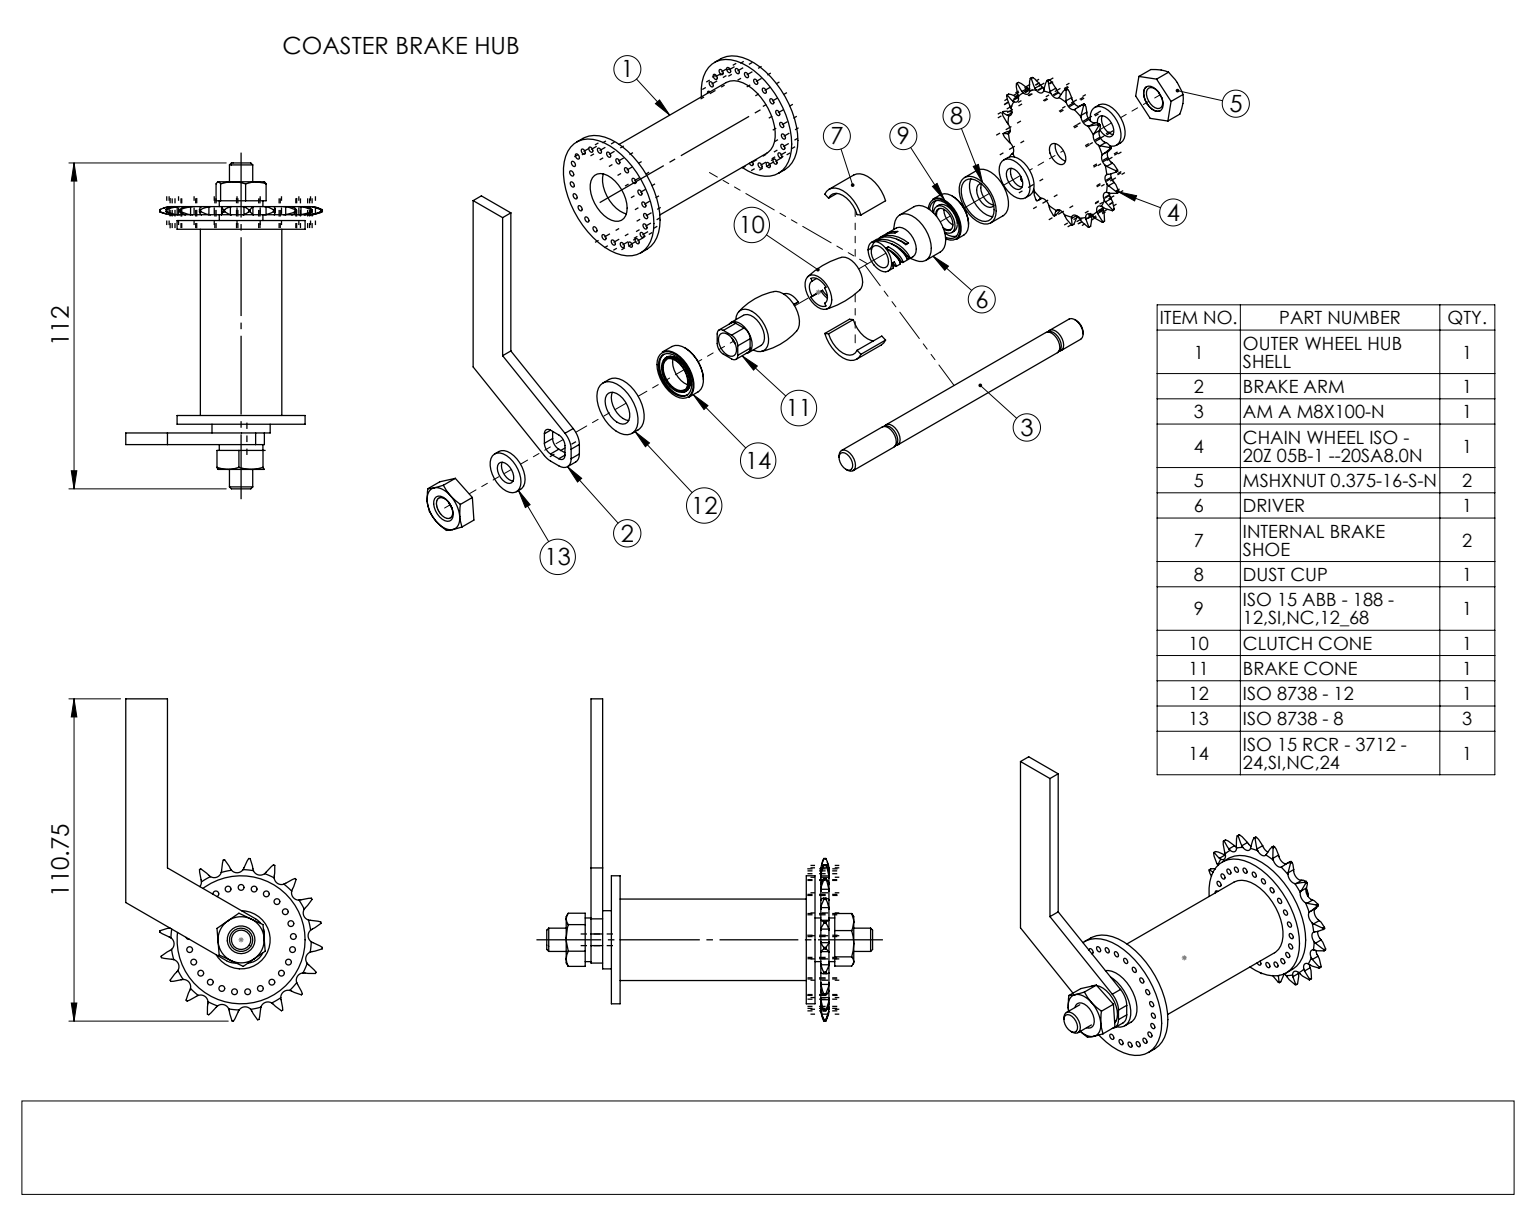
ISO-10303-21;
HEADER;
FILE_DESCRIPTION (('STEP AP214'),
    '1' );
FILE_NAME ('BR-591',
    '2026-10-08T05:56:58',
    ( '' ),
    ( '' ),
    'SwSTEP 2.0',
    'SolidWorks 2026',
    '' );
FILE_SCHEMA (( 'AUTOMOTIVE_DESIGN' ));
ENDSEC;

DATA;
#1 = ORIENTED_EDGE ( 'NONE', *, *, #18394, .T. ) ;
#2 = CARTESIAN_POINT ( 'NONE',  ( 0.07186808533286707934, 10.24630254990548650, -23.19485392143201707 ) ) ;
#3 = AXIS2_PLACEMENT_3D ( 'NONE', #18095, #1186, #4385 ) ;
#4 = FACE_OUTER_BOUND ( 'NONE', #5916, .T. ) ;
#5 = VECTOR ( 'NONE', #6897, 1000.000000000000000 ) ;
#6 = ORIENTED_EDGE ( 'NONE', *, *, #9270, .F. ) ;
#7 = CARTESIAN_POINT ( 'NONE',  ( 9.343749997951615427, -3.499494075959840966, 3.499494075959791672 ) ) ;
#8 = EDGE_CURVE ( 'NONE', #13643, #9700, #6131, .T. ) ;
#9 = CARTESIAN_POINT ( 'NONE',  ( 2.257825462012207574, 23.74442027961379864, -12.96514671151741638 ) ) ;
#10 = ORIENTED_EDGE ( 'NONE', *, *, #9147, .T. ) ;
#11 = ADVANCED_FACE ( 'NONE', ( #15453 ), #13841, .T. ) ;
#12 = CARTESIAN_POINT ( 'NONE',  ( 1.510506337161861223, 4.648860486681953397, -12.84374999795161543 ) ) ;
#13 = CARTESIAN_POINT ( 'NONE',  ( -15.00000000000000355, 4.874999999999997335, -3.903123748999000053 ) ) ;
#14 = ADVANCED_FACE ( 'NONE', ( #14340, #12840 ), #18938, .T. ) ;
#15 = VERTEX_POINT ( 'NONE', #17446 ) ;
#16 = VECTOR ( 'NONE', #6986, 1000.000000000000000 ) ;
#17 = B_SPLINE_CURVE_WITH_KNOTS ( 'NONE', 3,
 ( #2444, #6941, #2258, #8559, #14668, #14761 ),
 .UNSPECIFIED., .F., .F.,
 ( 4, 2, 4 ),
 ( 4.462636731831954487E-07, 0.001879885066974966781, 0.003759323870276750149 ),
 .UNSPECIFIED. ) ;
#18 = CARTESIAN_POINT ( 'NONE',  ( 12.84374999795161543, 1.016293382781411792, 4.781284448697195266 ) ) ;
#19 = CARTESIAN_POINT ( 'NONE',  ( 2.789999999999999147, -23.17675759782046541, 7.772527002114348882 ) ) ;
#20 = EDGE_LOOP ( 'NONE', ( #15641, #11996, #7928, #5193 ) ) ;
#21 = CARTESIAN_POINT ( 'NONE',  ( -14.19790265903626647, 9.644882309621941374, 35.00000000000000000 ) ) ;
#22 = VERTEX_POINT ( 'NONE', #14244 ) ;
#23 = CARTESIAN_POINT ( 'NONE',  ( -5.313169144388804277, -6.097875887622428159, -0.08160424337824753738 ) ) ;
#24 = ORIENTED_EDGE ( 'NONE', *, *, #5256, .T. ) ;
#25 = CYLINDRICAL_SURFACE ( 'NONE', #12194, 5.400000000000000355 ) ;
#26 = ADVANCED_FACE ( 'NONE', ( #15747 ), #18840, .T. ) ;
#27 = DIRECTION ( 'NONE',  ( 0.000000000000000000, 0.000000000000000000, 1.000000000000000000 ) ) ;
#28 = CARTESIAN_POINT ( 'NONE',  ( -10.58013454126452224, -14.56230589874905235, 32.00000000000000000 ) ) ;
#29 = CARTESIAN_POINT ( 'NONE',  ( -41.99999999999999289, -2.000000000000001776, 5.000000000000000000 ) ) ;
#30 = ORIENTED_EDGE ( 'NONE', *, *, #18526, .T. ) ;
#31 = CARTESIAN_POINT ( 'NONE',  ( 2.789999999999999147, -24.34211360614294506, -7.909232158575071558 ) ) ;
#32 =( BOUNDED_CURVE ( )  B_SPLINE_CURVE ( 2, ( #2369, #8482, #14588, #875, #19172, #5461, #16578, #8772, #11868, #7343, #19367, #11771, #17980, #5752, #6052 ),
 .UNSPECIFIED., .F., .F. ) 
 B_SPLINE_CURVE_WITH_KNOTS ( ( 3, 2, 2, 2, 2, 2, 2, 3 ),
 ( 0.000000000000000000, 0.05000000000000000278, 0.1000000000000000056, 0.1499999999999999944, 0.2000000000000000111, 0.2500000000000000000, 0.2999999999999999889, 0.3333180920165871863 ),
 .UNSPECIFIED. ) 
 CURVE ( )  GEOMETRIC_REPRESENTATION_ITEM ( )  RATIONAL_B_SPLINE_CURVE ( ( 1.000000000000000000, 0.9876883405951377704, 1.000000000000000000, 0.9876883405951377704, 1.000000000000000000, 0.9876883405951377704, 1.000000000000000000, 0.9876883405951377704, 1.000000000000000000, 0.9876883405951377704, 1.000000000000000000, 0.9876883405951377704, 1.000000000000000000, 0.9917959799814384247, 0.9945256517182510247 ) ) 
 REPRESENTATION_ITEM ( '' )  );
#33 = AXIS2_PLACEMENT_3D ( 'NONE', #19448, #5737, #11851 ) ;
#34 =( REPRESENTATION_RELATIONSHIP ('NONE','NONE', #18211, #17568 ) REPRESENTATION_RELATIONSHIP_WITH_TRANSFORMATION ( #11544 )SHAPE_REPRESENTATION_RELATIONSHIP( ) );
#35 = ADVANCED_FACE ( 'NONE', ( #2227 ), #2033, .F. ) ;
#36 = SURFACE_STYLE_FILL_AREA ( #16650 ) ;
#37 = CARTESIAN_POINT ( 'NONE',  ( -5.207209108562804722, 2.318398865532109276, -15.31249999590322552 ) ) ;
#38 = CARTESIAN_POINT ( 'NONE',  ( 15.28688694438835505, -7.664027248171309203, -32.00000000000000000 ) ) ;
#39 = DIRECTION ( 'NONE',  ( -1.000000000000000000, -0.000000000000000000, -0.000000000000000000 ) ) ;
#40 = ORIENTED_EDGE ( 'NONE', *, *, #11273, .T. ) ;
#41 = DIRECTION ( 'NONE',  ( 0.000000000000000000, 1.224646799147353454E-16, 1.000000000000000000 ) ) ;
#42 = ADVANCED_FACE ( 'NONE', ( #15944 ), #11240, .F. ) ;
#43 = DIRECTION ( 'NONE',  ( 1.000000000000000000, 0.000000000000000000, 0.000000000000000000 ) ) ;
#44 = ORIENTED_EDGE ( 'NONE', *, *, #4692, .F. ) ;
#45 = DIRECTION ( 'NONE',  ( 0.000000000000000000, 0.000000000000000000, -1.000000000000000000 ) ) ;
#46 = VECTOR ( 'NONE', #13444, 1000.000000000000000 ) ;
#47 = DIRECTION ( 'NONE',  ( 1.000000000000000000, 0.000000000000000000, 0.000000000000000000 ) ) ;
#48 = AXIS2_PLACEMENT_3D ( 'NONE', #1489, #16900, #7577 ) ;
#49 = DIRECTION ( 'NONE',  ( 0.000000000000000000, 0.000000000000000000, -1.000000000000000000 ) ) ;
#50 = CARTESIAN_POINT ( 'NONE',  ( -1.493657965219562511, -5.574407415329147852, -9.812499995903225525 ) ) ;
#51 = EDGE_CURVE ( 'NONE', #4769, #2089, #9336, .T. ) ;
#52 = CIRCLE ( 'NONE', #15065, 1.000000000000004441 ) ;
#53 = EDGE_LOOP ( 'NONE', ( #13652, #15680, #15664, #19409 ) ) ;
#54 = ORIENTED_EDGE ( 'NONE', *, *, #11125, .T. ) ;
#55 = CARTESIAN_POINT ( 'NONE',  ( 0.1882238782932349475, -17.47009390565476750, -19.18368891937510412 ) ) ;
#56 = CARTESIAN_POINT ( 'NONE',  ( 12.34374999795161543, 4.888101187500000222, 0.7741991708318884946 ) ) ;
#57 = ORIENTED_EDGE ( 'NONE', *, *, #11077, .F. ) ;
#58 = B_SPLINE_CURVE_WITH_KNOTS ( 'NONE', 3,
 ( #4738, #3235, #18159, #5934, #19743, #13850 ),
 .UNSPECIFIED., .F., .F.,
 ( 4, 2, 4 ),
 ( 4.462636882236601199E-07, 0.001879885203074806947, 0.003759324142461389993 ),
 .UNSPECIFIED. ) ;
#59 = VERTEX_POINT ( 'NONE', #14445 ) ;
#60 = FILL_AREA_STYLE ('',( #15279 ) ) ;
#61 = AXIS2_PLACEMENT_3D ( 'NONE', #11825, #841, #14548 ) ;
#62 = VERTEX_POINT ( 'NONE', #2132 ) ;
#63 = CIRCLE ( 'NONE', #5149, 40.00000000000000711 ) ;
#64 = VECTOR ( 'NONE', #5510, 1000.000000000000000 ) ;
#65 = AXIS2_PLACEMENT_3D ( 'NONE', #16794, #19682, #3071 ) ;
#66 = DIRECTION ( 'NONE',  ( -1.000000000000000000, 0.000000000000000000, 0.000000000000000000 ) ) ;
#67 = DIRECTION ( 'NONE',  ( -1.000000000000000000, 0.000000000000000000, 0.000000000000000000 ) ) ;
#68 = DIRECTION ( 'NONE',  ( 1.000000000000000000, 0.000000000000000000, 0.000000000000000000 ) ) ;
#69 = ORIENTED_EDGE ( 'NONE', *, *, #7451, .F. ) ;
#70 = ORIENTED_EDGE ( 'NONE', *, *, #8344, .T. ) ;
#71 = B_SPLINE_CURVE_WITH_KNOTS ( 'NONE', 3,
 ( #7909, #17128, #18622, #4920 ),
 .UNSPECIFIED., .F., .F.,
 ( 4, 4 ),
 ( 0.005258110598983589158, 0.005948376585272731332 ),
 .UNSPECIFIED. ) ;
#72 = CARTESIAN_POINT ( 'NONE',  ( 0.02436607992776411782, 22.71065055754465689, -9.836394144775473691 ) ) ;
#73 = DIRECTION ( 'NONE',  ( -1.000000000000000000, 0.000000000000000000, 0.000000000000000000 ) ) ;
#74 = EDGE_CURVE ( 'NONE', #13547, #344, #8025, .T. ) ;
#75 = ORIENTED_EDGE ( 'NONE', *, *, #12842, .F. ) ;
#76 = CARTESIAN_POINT ( 'NONE',  ( 2.789999999999999147, 19.64056340710875048, -14.55412442567624609 ) ) ;
#77 = AXIS2_PLACEMENT_3D ( 'NONE', #8605, #16216, #8311 ) ;
#78 = FACE_BOUND ( 'NONE', #16173, .T. ) ;
#79 = AXIS2_PLACEMENT_3D ( 'NONE', #11870, #19566, #2860 ) ;
#80 = CARTESIAN_POINT ( 'NONE',  ( 2.789999999999999147, -15.04425356660744839, -18.18163861606288378 ) ) ;
#81 = AXIS2_PLACEMENT_3D ( 'NONE', #18484, #1485, #6266 ) ;
#82 = CARTESIAN_POINT ( 'NONE',  ( 2.765633920072239516, 21.30679549418631780, 12.59161484032919986 ) ) ;
#83 = CARTESIAN_POINT ( 'NONE',  ( -4.620319390059805187, 1.773574444220790136, -11.34374999795161543 ) ) ;
#84 = EDGE_CURVE ( 'NONE', #8438, #18497, #5035, .T. ) ;
#85 = ORIENTED_EDGE ( 'NONE', *, *, #1576, .T. ) ;
#86 = DIRECTION ( 'NONE',  ( -0.9340060080012921873, 4.375140065418248206E-17, -0.3572572980605013271 ) ) ;
#87 = VECTOR ( 'NONE', #9663, 1000.000000000000000 ) ;
#88 = DIRECTION ( 'NONE',  ( 0.000000000000000000, 0.000000000000000000, -1.000000000000000000 ) ) ;
#89 = ORIENTED_EDGE ( 'NONE', *, *, #3339, .T. ) ;
#90 = PLANE ( 'NONE',  #2084 ) ;
#91 = CARTESIAN_POINT ( 'NONE',  ( 13.34374999795161365, -0.2590123213420631454, -4.942249507334558700 ) ) ;
#92 = AXIS2_PLACEMENT_3D ( 'NONE', #12278, #16979, #66 ) ;
#93 = EDGE_CURVE ( 'NONE', #2524, #1421, #17025, .T. ) ;
#94 = CARTESIAN_POINT ( 'NONE',  ( 8.468749997951615427, -1.988169868018530462, -4.465502636338051445 ) ) ;
#95 = DIRECTION ( 'NONE',  ( -1.000000000000000000, -0.000000000000000000, 0.000000000000000000 ) ) ;
#96 = ORIENTED_EDGE ( 'NONE', *, *, #17923, .T. ) ;
#97 = AXIS2_PLACEMENT_3D ( 'NONE', #19744, #12155, #18353 ) ;
#98 = CARTESIAN_POINT ( 'NONE',  ( 0.000000000000000000, 0.000000000000000000, -35.00000000000000000 ) ) ;
#99 = CYLINDRICAL_SURFACE ( 'NONE', #7805, 22.00000000000000355 ) ;
#100 = AXIS2_PLACEMENT_3D ( 'NONE', #5188, #8093, #8295 ) ;
#101 = CARTESIAN_POINT ( 'NONE',  ( 1.749999999999998002, -12.52377138324241734, 25.12109765559649688 ) ) ;
#102 = ORIENTED_EDGE ( 'NONE', *, *, #9565, .F. ) ;
#103 = CARTESIAN_POINT ( 'NONE',  ( -2.000000000000001776, 3.950217066951266176, 3.681818181818181213 ) ) ;
#104 = CARTESIAN_POINT ( 'NONE',  ( 11.46874999795161543, -2.444050593750019651, 4.233219804643871598 ) ) ;
#105 = CARTESIAN_POINT ( 'NONE',  ( 10.50000000000000711, 3.631840208645794821, 4.484949146646379781 ) ) ;
#106 = FACE_OUTER_BOUND ( 'NONE', #19772, .T. ) ;
#107 = EDGE_LOOP ( 'NONE', ( #13060, #5147, #11835, #11833, #16317, #5831 ) ) ;
#108 = CARTESIAN_POINT ( 'NONE',  ( 0.000000000000000000, 0.000000000000000000, 35.00000000000000000 ) ) ;
#109 = PRESENTATION_LAYER_ASSIGNMENT (  '', '', ( #8729 ) ) ;
#110 = CARTESIAN_POINT ( 'NONE',  ( 17.11901729331276556, 5.562305898749055011, -32.00000000000000000 ) ) ;
#111 = EDGE_CURVE ( 'NONE', #18625, #19430, #2327, .T. ) ;
#112 = EDGE_LOOP ( 'NONE', ( #14976, #17083 ) ) ;
#113 = FACE_OUTER_BOUND ( 'NONE', #17596, .T. ) ;
#114 = DIRECTION ( 'NONE',  ( -1.000000000000000000, -0.000000000000000000, -0.000000000000000000 ) ) ;
#115 = ORIENTED_EDGE ( 'NONE', *, *, #15621, .F. ) ;
#116 = AXIS2_PLACEMENT_3D ( 'NONE', #3393, #4893, #17196 ) ;
#117 = CARTESIAN_POINT ( 'NONE',  ( 1.749999999999998002, -4.633866840648726004, -27.68468304288263582 ) ) ;
#118 = CARTESIAN_POINT ( 'NONE',  ( -34.92499999999994742, 0.000000000000000000, 4.000000000000000000 ) ) ;
#119 = ORIENTED_EDGE ( 'NONE', *, *, #8237, .F. ) ;
#120 =( GEOMETRIC_REPRESENTATION_CONTEXT ( 3 ) GLOBAL_UNCERTAINTY_ASSIGNED_CONTEXT ( ( #987 ) ) GLOBAL_UNIT_ASSIGNED_CONTEXT ( ( #1597, #16819, #7588 ) ) REPRESENTATION_CONTEXT ( 'NONE', 'WORKASPACE' ) );
#121 = LINE ( 'NONE', #4819, #1475 ) ;
#122 = CARTESIAN_POINT ( 'NONE',  ( -34.92499999999994742, 0.000000000000000000, 0.000000000000000000 ) ) ;
#123 = VERTEX_POINT ( 'NONE', #15646 ) ;
#124 = EDGE_CURVE ( 'NONE', #6609, #1230, #1374, .T. ) ;
#125 = DIRECTION ( 'NONE',  ( -1.000000000000000000, -0.000000000000000000, -0.000000000000000000 ) ) ;
#126 = VERTEX_POINT ( 'NONE', #442 ) ;
#127 = EDGE_CURVE ( 'NONE', #15888, #11336, #18737, .T. ) ;
#128 = DIRECTION ( 'NONE',  ( 0.000000000000000000, 0.000000000000000000, 1.000000000000000000 ) ) ;
#129 = ORIENTED_EDGE ( 'NONE', *, *, #9030, .F. ) ;
#130 = DIRECTION ( 'NONE',  ( 1.000000000000000000, 0.000000000000000000, 0.000000000000000000 ) ) ;
#131 = AXIS2_PLACEMENT_3D ( 'NONE', #16442, #16336, #16243 ) ;
#132 = CARTESIAN_POINT ( 'NONE',  ( 2.631259771887293653, -22.38003579136350396, 12.81821841996065636 ) ) ;
#133 = DIRECTION ( 'NONE',  ( 1.000000000000000000, 0.000000000000000000, 0.000000000000000000 ) ) ;
#134 = EDGE_CURVE ( 'NONE', #16351, #5756, #19323, .T. ) ;
#135 = CARTESIAN_POINT ( 'NONE',  ( 0.1855656748306462045, -2.851997810081830842, 25.77772010606605235 ) ) ;
#136 = ORIENTED_EDGE ( 'NONE', *, *, #8190, .F. ) ;
#137 = DIRECTION ( 'NONE',  ( 0.000000000000000000, 0.000000000000000000, 1.000000000000000000 ) ) ;
#138 = PRESENTATION_LAYER_ASSIGNMENT (  '', '', ( #11327 ) ) ;
#139 = AXIS2_PLACEMENT_3D ( 'NONE', #2060, #12472, #13976 ) ;
#140 = LINE ( 'NONE', #6221, #2071 ) ;
#141 = EDGE_LOOP ( 'NONE', ( #3157, #7243, #2430, #12729, #17262, #10969 ) ) ;
#142 = VECTOR ( 'NONE', #16132, 1000.000000000000000 ) ;
#143 = DIRECTION ( 'NONE',  ( -0.000000000000000000, -0.000000000000000000, 1.000000000000000000 ) ) ;
#144 = CARTESIAN_POINT ( 'NONE',  ( 2.790000000000076419, -22.38018801136469094, -9.515416771311432598 ) ) ;
#145 = ORIENTED_EDGE ( 'NONE', *, *, #8344, .F. ) ;
#146 = CARTESIAN_POINT ( 'NONE',  ( 13.00000000000000533, 0.5958122406256767256, -5.668774803599153422 ) ) ;
#147 = CARTESIAN_POINT ( 'NONE',  ( 10.34374999795161543, 0.2590123213421660631, -4.942249507334553371 ) ) ;
#148 = ORIENTED_EDGE ( 'NONE', *, *, #16940, .F. ) ;
#149 = DIRECTION ( 'NONE',  ( 1.000000000000000000, 0.000000000000000000, -0.000000000000000000 ) ) ;
#150 = STYLED_ITEM ( 'NONE', ( #8512 ), #9431 ) ;
#151 = ORIENTED_EDGE ( 'NONE', *, *, #9100, .T. ) ;
#152 = SHAPE_DEFINITION_REPRESENTATION ( #11949, #13463 ) ;
#153 = CARTESIAN_POINT ( 'NONE',  ( 1.545624935189822177E-15, 9.165435523385314198, -6.527800000000000047 ) ) ;
#154 = CARTESIAN_POINT ( 'NONE',  ( -5.700000000000001066, -0.5990941410143296730, -13.64430100820692537 ) ) ;
#155 = VERTEX_POINT ( 'NONE', #3633 ) ;
#156 =( BOUNDED_SURFACE ( )  B_SPLINE_SURFACE ( 1, 2, ( 
 ( #19696, #12102, #10210, #2584, #16407, #18204, #1100, #2682, #8800, #7272, #189, #18685, #7680, #9499, #382, #3485, #10992 ),
 ( #15499, #9592, #10894, #9295, #13794, #4787, #17096, #10700, #6275, #4590, #15690, #10794, #17000, #15330, #18396, #284, #6461 ) ),
 .UNSPECIFIED., .F., .F., .F. ) 
 B_SPLINE_SURFACE_WITH_KNOTS ( ( 2, 2 ),
 ( 3, 2, 2, 2, 2, 2, 2, 2, 3 ),
 ( 0.000000000000000000, 1.000000000000000000 ),
 ( 0.000000000000000000, 0.05000000000000000278, 0.1000000000000000056, 0.1499999999999999944, 0.2000000000000000111, 0.2500000000000000000, 0.2999999999999999889, 0.3499999999999999778, 0.4000000000000000222 ),
 .UNSPECIFIED. ) 
 GEOMETRIC_REPRESENTATION_ITEM ( )  RATIONAL_B_SPLINE_SURFACE ( (
 ( 1.000000000000000000, 0.9876883405951377704, 1.000000000000000000, 0.9876883405951377704, 1.000000000000000000, 0.9876883405951377704, 1.000000000000000000, 0.9876883405951377704, 1.000000000000000000, 0.9876883405951377704, 1.000000000000000000, 0.9876883405951377704, 1.000000000000000000, 0.9876883405951377704, 1.000000000000000000, 0.9876883405951377704, 1.000000000000000000),
 ( 1.000000000000000000, 0.9876883405951377704, 1.000000000000000000, 0.9876883405951377704, 1.000000000000000000, 0.9876883405951377704, 1.000000000000000000, 0.9876883405951377704, 1.000000000000000000, 0.9876883405951377704, 1.000000000000000000, 0.9876883405951377704, 1.000000000000000000, 0.9876883405951377704, 1.000000000000000000, 0.9876883405951377704, 1.000000000000000000) ) ) 
 REPRESENTATION_ITEM ( '' )  SURFACE ( )  );
#157 = ORIENTED_EDGE ( 'NONE', *, *, #10548, .F. ) ;
#158 = CARTESIAN_POINT ( 'NONE',  ( -0.8944271909999155223, 0.000000000000000000, 0.000000000000000000 ) ) ;
#159 = CARTESIAN_POINT ( 'NONE',  ( 4.465502636338025688, -1.988169868018592412, -14.84374999795161543 ) ) ;
#161 = EDGE_LOOP ( 'NONE', ( #14576, #14310, #4192, #11228 ) ) ;
#160 = AXIS2_PLACEMENT_3D ( 'NONE', #12502, #14297, #392 ) ;
#162 = EDGE_CURVE ( 'NONE', #18627, #6765, #11284, .T. ) ;
#163 = EDGE_CURVE ( 'NONE', #5395, #4220, #13751, .T. ) ;
#164 = CYLINDRICAL_SURFACE ( 'NONE', #11252, 13.19999999999999929 ) ;
#165 = VECTOR ( 'NONE', #11258, 1000.000000000000000 ) ;
#166 = ORIENTED_EDGE ( 'NONE', *, *, #11587, .F. ) ;
#167 = EDGE_CURVE ( 'NONE', #11813, #19442, #2963, .T. ) ;
#168 = FACE_OUTER_BOUND ( 'NONE', #5426, .T. ) ;
#169 = CARTESIAN_POINT ( 'NONE',  ( 5.421022142882364392, -1.761396867937238486, -8.312499995903225525 ) ) ;
#170 = EDGE_CURVE ( 'NONE', #2370, #11052, #11954, .T. ) ;
#171 = ORIENTED_EDGE ( 'NONE', *, *, #6016, .T. ) ;
#172 = ORIENTED_EDGE ( 'NONE', *, *, #5127, .T. ) ;
#173 = CARTESIAN_POINT ( 'NONE',  ( -7.634507448887241432E-14, 22.38018801136490055, -9.515416771310970745 ) ) ;
#174 = EDGE_CURVE ( 'NONE', #16744, #5554, #14796, .T. ) ;
#175 = CARTESIAN_POINT ( 'NONE',  ( 6.234374998975811266, 0.000000000000000000, -5.294050593750000644 ) ) ;
#176 = ORIENTED_EDGE ( 'NONE', *, *, #9057, .T. ) ;
#177 = EDGE_LOOP ( 'NONE', ( #14869, #8807, #10159, #6951 ) ) ;
#178 = LINE ( 'NONE', #6262, #6325 ) ;
#179 = VECTOR ( 'NONE', #5539, 1000.000000000000000 ) ;
#180 = CARTESIAN_POINT ( 'NONE',  ( -5.387740456496247887, -2.068159791354146293, -12.81249999590322552 ) ) ;
#181 = CARTESIAN_POINT ( 'NONE',  ( 8.000000000000000000, 0.000000000000000000, 0.000000000000000000 ) ) ;
#182 = AXIS2_PLACEMENT_3D ( 'NONE', #8021, #14038, #15743 ) ;
#183 = DIRECTION ( 'NONE',  ( 0.000000000000000000, 0.000000000000000000, 1.000000000000000000 ) ) ;
#184 = CARTESIAN_POINT ( 'NONE',  ( 2.246813503491833508, 4.409619785863906571, -12.96874999795161543 ) ) ;
#185 = ORIENTED_EDGE ( 'NONE', *, *, #222, .T. ) ;
#186 = CARTESIAN_POINT ( 'NONE',  ( 7.843749997951614539, -3.270778111535287191, -3.632567103900569361 ) ) ;
#187 = DIRECTION ( 'NONE',  ( 0.000000000000000000, 0.000000000000000000, -1.000000000000000000 ) ) ;
#188 = ORIENTED_EDGE ( 'NONE', *, *, #15203, .F. ) ;
#189 = CARTESIAN_POINT ( 'NONE',  ( 11.46874999795161543, 2.444050593750049405, -4.233219804643852946 ) ) ;
#190 = EDGE_CURVE ( 'NONE', #10991, #3279, #7426, .T. ) ;
#191 = CARTESIAN_POINT ( 'NONE',  ( 1.039999999999997593, 0.000000000000000000, 0.000000000000000000 ) ) ;
#192 = AXIS2_PLACEMENT_3D ( 'NONE', #8954, #15156, #10755 ) ;
#193 = AXIS2_PLACEMENT_3D ( 'NONE', #6002, #12326, #18419 ) ;
#194 = DIRECTION ( 'NONE',  ( -1.000000000000000000, -0.000000000000000000, 0.000000000000000000 ) ) ;
#195 = CARTESIAN_POINT ( 'NONE',  ( 12.86923836996420967, -11.47363181547641453, 32.00000000000000000 ) ) ;
#196 = VERTEX_POINT ( 'NONE', #4350 ) ;
#197 = EDGE_CURVE ( 'NONE', #5418, #16213, #1053, .T. ) ;
#198 = CARTESIAN_POINT ( 'NONE',  ( -2.000000000000000000, 1.999999999999998224, 41.99999999999999289 ) ) ;
#199 = SURFACE_SIDE_STYLE ('',( #8289 ) ) ;
#200 = DIRECTION ( 'NONE',  ( 0.000000000000000000, 0.000000000000000000, 1.000000000000000000 ) ) ;
#201 = VERTEX_POINT ( 'NONE', #5838 ) ;
#202 = DIRECTION ( 'NONE',  ( -1.000000000000000000, -0.000000000000000000, -0.000000000000000000 ) ) ;
#203 = CARTESIAN_POINT ( 'NONE',  ( 13.46874999795161543, -4.465502636338038123, 1.988169868018562880 ) ) ;
#204 = LINE ( 'NONE', #3197, #2253 ) ;
#205 = DIRECTION ( 'NONE',  ( 1.000000000000000000, 0.000000000000000000, 0.000000000000000000 ) ) ;
#206 = ORIENTED_EDGE ( 'NONE', *, *, #1733, .T. ) ;
#207 = CARTESIAN_POINT ( 'NONE',  ( -41.99999999999999289, -2.000000000000001776, -2.000000000000000000 ) ) ;
#208 = CIRCLE ( 'NONE', #5304, 6.000000000000021316 ) ;
#209 = ADVANCED_FACE ( 'NONE', ( #15358 ), #16764, .F. ) ;
#210 = CARTESIAN_POINT ( 'NONE',  ( -2.000000000000001776, 3.218695387886217674, 2.999999999999999556 ) ) ;
#211 = AXIS2_PLACEMENT_3D ( 'NONE', #17804, #14615, #6883 ) ;
#212 = ORIENTED_EDGE ( 'NONE', *, *, #10668, .T. ) ;
#213 = CARTESIAN_POINT ( 'NONE',  ( 14.84374999795161543, -2.873153789725797935, -3.954556930911881096 ) ) ;
#214 = CARTESIAN_POINT ( 'NONE',  ( 3.954556930911861112, 2.873153789725825913, -14.84374999795161543 ) ) ;
#215 = ORIENTED_EDGE ( 'NONE', *, *, #17541, .F. ) ;
#216 = EDGE_CURVE ( 'NONE', #1617, #5986, #4540, .T. ) ;
#217 = CARTESIAN_POINT ( 'NONE',  ( -1.310841663519413114, 4.898587196589412829E-16, -4.000000000000000000 ) ) ;
#218 = ORIENTED_EDGE ( 'NONE', *, *, #8182, .T. ) ;
#219 = CIRCLE ( 'NONE', #8203, 1.000000000000000888 ) ;
#220 = DIRECTION ( 'NONE',  ( 1.000000000000000000, 0.000000000000000000, 0.000000000000000000 ) ) ;
#221 = CARTESIAN_POINT ( 'NONE',  ( -4.888101187500000222, 0.7741991708318887166, -6.968749997951614539 ) ) ;
#222 = EDGE_CURVE ( 'NONE', #241, #19442, #19105, .T. ) ;
#223 = VECTOR ( 'NONE', #15319, 1000.000000000000114 ) ;
#224 = EDGE_LOOP ( 'NONE', ( #18143, #6308, #7180, #10221, #12160, #16054 ) ) ;
#225 = CARTESIAN_POINT ( 'NONE',  ( 2.500000000000002220, 0.000000000000000000, 0.000000000000000000 ) ) ;
#226 = VERTEX_POINT ( 'NONE', #15455 ) ;
#227 = CARTESIAN_POINT ( 'NONE',  ( 0.02436607992776325046, -24.15498966839958683, -5.391175441198872598 ) ) ;
#228 = EDGE_LOOP ( 'NONE', ( #8346, #6074 ) ) ;
#229 = DIRECTION ( 'NONE',  ( -1.000000000000000000, 0.000000000000000000, 0.000000000000000000 ) ) ;
#230 = CARTESIAN_POINT ( 'NONE',  ( -3.270778111535363131, -3.632567103900500971, -10.84374999795161543 ) ) ;
#231 = CARTESIAN_POINT ( 'NONE',  ( 2.444050593750020095, 4.233219804643871598, -6.468749997951615427 ) ) ;
#232 = CARTESIAN_POINT ( 'NONE',  ( 4.942249507334556036, -0.2590123213421313686, -9.968749997951617203 ) ) ;
#233 = ORIENTED_EDGE ( 'NONE', *, *, #5523, .T. ) ;
#234 = CARTESIAN_POINT ( 'NONE',  ( 4.200000000000000178, 0.000000000000000000, -28.99999999999999645 ) ) ;
#235 = CIRCLE ( 'NONE', #5349, 0.1999999999999996503 ) ;
#236 = DIRECTION ( 'NONE',  ( 1.000000000000000000, 0.000000000000000000, 0.000000000000000000 ) ) ;
#237 = EDGE_CURVE ( 'NONE', #6503, #6248, #1744, .T. ) ;
#238 = ORIENTED_EDGE ( 'NONE', *, *, #5736, .T. ) ;
#239 = CARTESIAN_POINT ( 'NONE',  ( 2.790000000000000036, 20.85230829256853013, 12.51294990530023732 ) ) ;
#240 = DIRECTION ( 'NONE',  ( 0.000000000000000000, 0.000000000000000000, 1.000000000000000000 ) ) ;
#241 = VERTEX_POINT ( 'NONE', #6034 ) ;
#242 = CARTESIAN_POINT ( 'NONE',  ( 2.030753602223784871, 27.14986936243581184, -4.828194074574073902 ) ) ;
#243 = CARTESIAN_POINT ( 'NONE',  ( 8.843749997951615427, -1.988169868018530462, -4.465502636338051445 ) ) ;
#244 = ADVANCED_FACE ( 'NONE', ( #13550 ), #6454, .T. ) ;
#245 = ORIENTED_EDGE ( 'NONE', *, *, #12939, .T. ) ;
#246 = FACE_OUTER_BOUND ( 'NONE', #2374, .T. ) ;
#247 = VECTOR ( 'NONE', #10712, 1000.000000000000000 ) ;
#248 = ORIENTED_EDGE ( 'NONE', *, *, #1052, .F. ) ;
#249 = SHAPE_DEFINITION_REPRESENTATION ( #10039, #10045 ) ;
#250 = CARTESIAN_POINT ( 'NONE',  ( 0.02436607992776151574, 24.15498966839970052, -5.391175441198366336 ) ) ;
#251 = AXIS2_PLACEMENT_3D ( 'NONE', #17536, #9945, #11526 ) ;
#252 = CARTESIAN_POINT ( 'NONE',  ( 11.46874999795161543, 2.444050593749990785, 4.233219804643887585 ) ) ;
#253 = VERTEX_POINT ( 'NONE', #1447 ) ;
#254 = ORIENTED_EDGE ( 'NONE', *, *, #5488, .T. ) ;
#255 = CARTESIAN_POINT ( 'NONE',  ( 0.02436607992776411782, -16.37294372382844543, -18.55949924794910544 ) ) ;
#256 = CARTESIAN_POINT ( 'NONE',  ( 2.318398865532073749, 5.207209108562820710, -10.31249999590322552 ) ) ;
#257 = VERTEX_POINT ( 'NONE', #7635 ) ;
#258 = DIRECTION ( 'NONE',  ( 0.000000000000000000, 0.000000000000000000, 1.000000000000000000 ) ) ;
#259 = EDGE_CURVE ( 'NONE', #12604, #8838, #10645, .T. ) ;
#260 = AXIS2_PLACEMENT_3D ( 'NONE', #9213, #397, #16916 ) ;
#261 = ORIENTED_EDGE ( 'NONE', *, *, #7786, .T. ) ;
#262 = CARTESIAN_POINT ( 'NONE',  ( 2.789999999999999147, 24.15498966839970052, -5.391175441198366336 ) ) ;
#263 = EDGE_CURVE ( 'NONE', #17130, #17826, #3141, .T. ) ;
#264 = FACE_BOUND ( 'NONE', #19064, .T. ) ;
#265 = EDGE_CURVE ( 'NONE', #3536, #12799, #14477, .T. ) ;
#266 = EDGE_LOOP ( 'NONE', ( #427, #17181, #9017, #11698, #10341, #16603 ) ) ;
#267 = DIRECTION ( 'NONE',  ( 0.000000000000000000, 0.000000000000000000, 1.000000000000000000 ) ) ;
#268 =( NAMED_UNIT ( * ) PLANE_ANGLE_UNIT ( ) SI_UNIT ( $, .RADIAN. ) );
#269 = DIRECTION ( 'NONE',  ( 1.000000000000000000, 0.000000000000000000, 0.000000000000000000 ) ) ;
#270 = EDGE_LOOP ( 'NONE', ( #16817, #14274, #8811, #901, #1434 ) ) ;
#271 = VERTEX_POINT ( 'NONE', #7531 ) ;
#272 = CARTESIAN_POINT ( 'NONE',  ( 2.030753603471112889, -12.98165646470063983, -24.32906614999630790 ) ) ;
#273 = AXIS2_PLACEMENT_3D ( 'NONE', #16273, #13173, #8869 ) ;
#274 = CARTESIAN_POINT ( 'NONE',  ( -4.936344801571327601, -2.849999999999954792, -12.31249999590322552 ) ) ;
#275 = CARTESIAN_POINT ( 'NONE',  ( -5.668774803599153422, 0.5958122406256767256, -13.00000000000000533 ) ) ;
#276 = EDGE_CURVE ( 'NONE', #11279, #870, #9053, .T. ) ;
#277 = DIRECTION ( 'NONE',  ( 1.000000000000000000, 0.000000000000000000, 0.000000000000000000 ) ) ;
#278 = CARTESIAN_POINT ( 'NONE',  ( -4.409619785863906571, 2.246813503491833508, -7.968749997951616315 ) ) ;
#279 =( GEOMETRIC_REPRESENTATION_CONTEXT ( 3 ) GLOBAL_UNCERTAINTY_ASSIGNED_CONTEXT ( ( #18002 ) ) GLOBAL_UNIT_ASSIGNED_CONTEXT ( ( #11074, #12777, #13979 ) ) REPRESENTATION_CONTEXT ( 'NONE', 'WORKASPACE' ) );
#280 = ORIENTED_EDGE ( 'NONE', *, *, #9401, .T. ) ;
#281 = CARTESIAN_POINT ( 'NONE',  ( 1.394999999999999574, -19.67366047555515607, -20.02152543075367319 ) ) ;
#282 = DIRECTION ( 'NONE',  ( 1.000000000000000000, 0.000000000000000000, 0.000000000000000000 ) ) ;
#283 = VERTEX_POINT ( 'NONE', #13651 ) ;
#284 = CARTESIAN_POINT ( 'NONE',  ( 13.50000000000000533, 5.574407415329178939, -1.493657965219446382 ) ) ;
#286 = EDGE_CURVE ( 'NONE', #5172, #4659, #9375, .T. ) ;
#285 = EDGE_CURVE ( 'NONE', #19646, #4617, #17355, .T. ) ;
#287 = DIRECTION ( 'NONE',  ( 0.000000000000000000, 0.000000000000000000, 1.000000000000000000 ) ) ;
#288 = AXIS2_PLACEMENT_3D ( 'NONE', #4753, #9067, #13763 ) ;
#289 = CARTESIAN_POINT ( 'NONE',  ( 2.999999999999998224, -2.487173708821168283, 2.318181818181817455 ) ) ;
#290 = CYLINDRICAL_SURFACE ( 'NONE', #1072, 13.19999999999999929 ) ;
#291 = CARTESIAN_POINT ( 'NONE',  ( -6.403158385254602634E-17, -23.69843731927173991, 5.456805104201007950 ) ) ;
#292 = ORIENTED_EDGE ( 'NONE', *, *, #3282, .F. ) ;
#293 = DIRECTION ( 'NONE',  ( 1.000000000000000000, 0.000000000000000000, 0.000000000000000000 ) ) ;
#294 =( LENGTH_UNIT ( ) NAMED_UNIT ( * ) SI_UNIT ( .MILLI., .METRE. ) );
#295 = DIRECTION ( 'NONE',  ( -1.000000000000000000, 0.000000000000000000, 0.000000000000000000 ) ) ;
#296 = AXIS2_PLACEMENT_3D ( 'NONE', #14579, #867, #16469 ) ;
#297 = SURFACE_STYLE_FILL_AREA ( #4139 ) ;
#298 = VERTEX_POINT ( 'NONE', #551 ) ;
#299 = CARTESIAN_POINT ( 'NONE',  ( 7.312499995903225525, 4.936344801571308061, -2.849999999999989431 ) ) ;
#300 = CARTESIAN_POINT ( 'NONE',  ( -18.11901729331277267, 5.562305898749051458, 35.00000000000000000 ) ) ;
#301 = FACE_OUTER_BOUND ( 'NONE', #19198, .T. ) ;
#302 = CARTESIAN_POINT ( 'NONE',  ( 0.02436607992776325046, -18.55949924794904504, 16.37294372382852004 ) ) ;
#303 = VERTEX_POINT ( 'NONE', #15551 ) ;
#304 = LINE ( 'NONE', #1515, #19226 ) ;
#305 = CIRCLE ( 'NONE', #5078, 0.9999999999999974465 ) ;
#306 = CARTESIAN_POINT ( 'NONE',  ( -2.246813503491833508, 4.409619785863906571, -10.34374999795161543 ) ) ;
#307 = VERTEX_POINT ( 'NONE', #8239 ) ;
#308 = CARTESIAN_POINT ( 'NONE',  ( 8.500000000000005329, -1.493657965219446160, -5.574407415329178939 ) ) ;
#309 = B_SPLINE_CURVE_WITH_KNOTS ( 'NONE', 3,
 ( #72, #13681, #173, #13881 ),
 .UNSPECIFIED., .F., .F.,
 ( 4, 4 ),
 ( 3.059063720795852959E-07, 0.0006888942284914018055 ),
 .UNSPECIFIED. ) ;
#310 = CYLINDRICAL_SURFACE ( 'NONE', #17454, 1.000000000000000888 ) ;
#311 = CIRCLE ( 'NONE', #4137, 28.06981291497571007 ) ;
#312 = VERTEX_POINT ( 'NONE', #643 ) ;
#313 = CARTESIAN_POINT ( 'NONE',  ( 8.000000000000000000, 0.000000000000000000, 0.000000000000000000 ) ) ;
#314 = DIRECTION ( 'NONE',  ( 0.000000000000000000, 0.000000000000000000, -1.000000000000000000 ) ) ;
#315 = ORIENTED_EDGE ( 'NONE', *, *, #13010, .T. ) ;
#316 = CARTESIAN_POINT ( 'NONE',  ( -25.31088913245550032, 24.69615242270646149, 37.99999999999999289 ) ) ;
#317 = CYLINDRICAL_SURFACE ( 'NONE', #4942, 28.06981291497571362 ) ;
#318 = ORIENTED_EDGE ( 'NONE', *, *, #3578, .F. ) ;
#319 = CARTESIAN_POINT ( 'NONE',  ( 5.510910596163084625E-16, 18.00000000000000355, 32.00000000000000000 ) ) ;
#320 = ORIENTED_EDGE ( 'NONE', *, *, #14476, .T. ) ;
#321 = ORIENTED_EDGE ( 'NONE', *, *, #19741, .T. ) ;
#322 = TOROIDAL_SURFACE ( 'NONE', #2538, 6.200000000000021494, 0.2000000000000003164 ) ;
#323 = B_SPLINE_CURVE_WITH_KNOTS ( 'NONE', 3,
 ( #16486, #1173, #972, #14689 ),
 .UNSPECIFIED., .F., .F.,
 ( 4, 4 ),
 ( 0.005258120783916789796, 0.005948386350302923772 ),
 .UNSPECIFIED. ) ;
#324 = CIRCLE ( 'NONE', #2869, 2.524999999999995914 ) ;
#325 = CYLINDRICAL_SURFACE ( 'NONE', #16943, 1.000000000000000888 ) ;
#326 = B_SPLINE_CURVE_WITH_KNOTS ( 'NONE', 3,
 ( #1232, #13430, #19527, #11936, #18048, #15038 ),
 .UNSPECIFIED., .F., .F.,
 ( 4, 2, 4 ),
 ( 4.462636793144857890E-07, 0.001879885123570645663, 0.003759323983461976531 ),
 .UNSPECIFIED. ) ;
#327 = LINE ( 'NONE', #14033, #13965 ) ;
#328 = CARTESIAN_POINT ( 'NONE',  ( 4.465502636338039011, 1.988169868018562436, -8.468749997951615427 ) ) ;
#329 = CARTESIAN_POINT ( 'NONE',  ( 4.780397808154266848, 1.280903732194421218, -8.968749997951611874 ) ) ;
#330 = ORIENTED_EDGE ( 'NONE', *, *, #12182, .F. ) ;
#331 = CARTESIAN_POINT ( 'NONE',  ( 0.8291131470075423504, 24.44424927289185945, 12.96989951879416125 ) ) ;
#332 = DIRECTION ( 'NONE',  ( 0.000000000000000000, 0.000000000000000000, 1.000000000000000000 ) ) ;
#333 = EDGE_CURVE ( 'NONE', #18696, #7394, #11045, .T. ) ;
#334 = VECTOR ( 'NONE', #14992, 1000.000000000000000 ) ;
#335 = ORIENTED_EDGE ( 'NONE', *, *, #16315, .T. ) ;
#336 = COLOUR_RGB ( '', 0.08235294, 0.09019608, 0.10196078) ;
#337 = DIRECTION ( 'NONE',  ( 1.000000000000000000, 6.419766481290786633E-33, -0.000000000000000000 ) ) ;
#338 = DIRECTION ( 'NONE',  ( 0.000000000000000000, 0.000000000000000000, 1.000000000000000000 ) ) ;
#339 = ORIENTED_EDGE ( 'NONE', *, *, #167, .F. ) ;
#340 = CARTESIAN_POINT ( 'NONE',  ( -1.869200000000000195, 0.000000000000000000, -8.239200000000002078 ) ) ;
#341 = CARTESIAN_POINT ( 'NONE',  ( 5.510910596163084625E-16, 18.00000000000000355, -32.00000000000000000 ) ) ;
#342 = EDGE_LOOP ( 'NONE', ( #5793, #6421, #6456, #12755 ) ) ;
#343 = CYLINDRICAL_SURFACE ( 'NONE', #4937, 5.400000000000000355 ) ;
#344 = VERTEX_POINT ( 'NONE', #2135 ) ;
#345 = CARTESIAN_POINT ( 'NONE',  ( 6.843749997951615427, -3.413342815706642518E-14, 4.888101187500000222 ) ) ;
#346 = CARTESIAN_POINT ( 'NONE',  ( 14.34374999795161365, -1.280903732194453859, 4.780397808154257078 ) ) ;
#347 = ORIENTED_EDGE ( 'NONE', *, *, #1908, .F. ) ;
#348 = ORIENTED_EDGE ( 'NONE', *, *, #8508, .T. ) ;
#349 = CARTESIAN_POINT ( 'NONE',  ( 0.000000000000000000, 9.324097380959777581, -22.25075486061729535 ) ) ;
#350 = AXIS2_PLACEMENT_3D ( 'NONE', #15262, #4448, #9055 ) ;
#351 = FACE_OUTER_BOUND ( 'NONE', #6860, .T. ) ;
#352 = ORIENTED_EDGE ( 'NONE', *, *, #18069, .F. ) ;
#353 = EDGE_CURVE ( 'NONE', #3827, #6550, #12668, .T. ) ;
#354 = CARTESIAN_POINT ( 'NONE',  ( -3.270778111535288080, 3.632567103900569361, -12.84374999795161543 ) ) ;
#355 = ORIENTED_EDGE ( 'NONE', *, *, #12536, .T. ) ;
#356 = AXIS2_PLACEMENT_3D ( 'NONE', #1344, #12254, #12353 ) ;
#357 = CARTESIAN_POINT ( 'NONE',  ( 14.00000000000000178, 1.714505518806294835E-15, -32.00000000000000000 ) ) ;
#358 = AXIS2_PLACEMENT_3D ( 'NONE', #10152, #1142, #7214 ) ;
#359 = CARTESIAN_POINT ( 'NONE',  ( -11.00000000000000355, -4.215373648918917304, -3.375000000000002665 ) ) ;
#360 = FACE_OUTER_BOUND ( 'NONE', #7817, .T. ) ;
#361 = EDGE_LOOP ( 'NONE', ( #9949, #14872, #12238, #18808 ) ) ;
#362 = CARTESIAN_POINT ( 'NONE',  ( 18.68117051311639543, -3.372863662543048591, 35.00000000000000000 ) ) ;
#363 =( NAMED_UNIT ( * ) PLANE_ANGLE_UNIT ( ) SI_UNIT ( $, .RADIAN. ) );
#364 = ORIENTED_EDGE ( 'NONE', *, *, #11679, .T. ) ;
#365 = ADVANCED_FACE ( 'NONE', ( #12843 ), #6521, .F. ) ;
#366 = ORIENTED_EDGE ( 'NONE', *, *, #9892, .F. ) ;
#367 = CARTESIAN_POINT ( 'NONE',  ( -7.372183127218402931E-16, -20.85230829256862961, 12.51294990530008988 ) ) ;
#368 = ADVANCED_FACE ( 'NONE', ( #12448 ), #16395, .F. ) ;
#369 = CARTESIAN_POINT ( 'NONE',  ( 0.3020334839682081163, -5.763142191869158992, -8.812499995903225525 ) ) ;
#370 = CARTESIAN_POINT ( 'NONE',  ( 0.000000000000000000, 0.000000000000000000, -6.527800000000000047 ) ) ;
#371 = ADVANCED_FACE ( 'NONE', ( #7931 ), #17448, .F. ) ;
#372 = AXIS2_PLACEMENT_3D ( 'NONE', #16435, #19135, #4224 ) ;
#373 = CARTESIAN_POINT ( 'NONE',  ( -4.611396867937201272, 3.350375938067097437, -8.000000000000005329 ) ) ;
#374 = AXIS2_PLACEMENT_3D ( 'NONE', #709, #6787, #13013 ) ;
#375 = ORIENTED_EDGE ( 'NONE', *, *, #4815, .F. ) ;
#376 = CARTESIAN_POINT ( 'NONE',  ( 1.039999999999996483, -19.67366047555544384, 20.02152543075338897 ) ) ;
#377 = AXIS2_PLACEMENT_3D ( 'NONE', #4115, #10228, #19314 ) ;
#378 = EDGE_CURVE ( 'NONE', #12550, #10168, #4252, .T. ) ;
#379 = CARTESIAN_POINT ( 'NONE',  ( 7.343749997951615427, -0.7741991708319229115, 4.888101187499994893 ) ) ;
#380 = B_SPLINE_CURVE_WITH_KNOTS ( 'NONE', 3,
 ( #13281, #8977, #18084, #2664, #14786, #5762 ),
 .UNSPECIFIED., .F., .F.,
 ( 4, 2, 4 ),
 ( 2.380731676443570881E-07, 0.002318718087522258532, 0.004637198101876872751 ),
 .UNSPECIFIED. ) ;
#381 = ORIENTED_EDGE ( 'NONE', *, *, #16041, .F. ) ;
#382 = CARTESIAN_POINT ( 'NONE',  ( 13.46874999795161543, 4.465502636338051445, -1.988169868018530906 ) ) ;
#383 = LINE ( 'NONE', #6367, #16649 ) ;
#384 = CARTESIAN_POINT ( 'NONE',  ( 0.000000000000000000, -7.909232158574647009, -24.34211360614308006 ) ) ;
#385 = EDGE_CURVE ( 'NONE', #2370, #813, #18633, .T. ) ;
#386 = CARTESIAN_POINT ( 'NONE',  ( 5.668774803599163192, 0.5958122406255991210, -9.000000000000005329 ) ) ;
#387 = ORIENTED_EDGE ( 'NONE', *, *, #12742, .F. ) ;
#388 = AXIS2_PLACEMENT_3D ( 'NONE', #15598, #18590, #11093 ) ;
#389 = AXIS2_PLACEMENT_3D ( 'NONE', #8278, #3775, #11481 ) ;
#390 = CARTESIAN_POINT ( 'NONE',  ( -6.626241948324210540, -16.73597674598852336, 32.00000000000000000 ) ) ;
#391 =( NAMED_UNIT ( * ) PLANE_ANGLE_UNIT ( ) SI_UNIT ( $, .RADIAN. ) );
#392 = DIRECTION ( 'NONE',  ( 1.000000000000000000, 0.000000000000000000, 0.000000000000000000 ) ) ;
#393 = VECTOR ( 'NONE', #16004, 1000.000000000000000 ) ;
#394 = DIRECTION ( 'NONE',  ( -1.000000000000000000, -0.000000000000000000, -0.000000000000000000 ) ) ;
#395 = EDGE_LOOP ( 'NONE', ( #14835, #13456, #12249, #10403 ) ) ;
#396 = PRODUCT_DEFINITION ( 'UNKNOWN', '', #3806, #10010 ) ;
#397 = DIRECTION ( 'NONE',  ( 0.5000000000000004441, -0.8660254037844383745, 0.000000000000000000 ) ) ;
#398 = CARTESIAN_POINT ( 'NONE',  ( 2.765633920072235963, -5.391175441198450713, -24.15498966839968276 ) ) ;
#399 = EDGE_CURVE ( 'NONE', #17067, #16866, #445, .T. ) ;
#400 = CARTESIAN_POINT ( 'NONE',  ( 6.468749997951615427, 4.233219804643887585, -2.444050593749990341 ) ) ;
#401 = CARTESIAN_POINT ( 'NONE',  ( 1.749999999999998002, 25.12109765559671004, -12.52377138324198391 ) ) ;
#402 = DIRECTION ( 'NONE',  ( 0.000000000000000000, 0.000000000000000000, -1.000000000000000000 ) ) ;
#403 = ORIENTED_EDGE ( 'NONE', *, *, #6295, .F. ) ;
#404 = CYLINDRICAL_SURFACE ( 'NONE', #4852, 1.000000000000004441 ) ;
#405 = DIRECTION ( 'NONE',  ( 1.000000000000000000, 0.000000000000000000, 0.000000000000000000 ) ) ;
#406 = EDGE_LOOP ( 'NONE', ( #6297, #10419, #12416, #16842 ) ) ;
#407 = CARTESIAN_POINT ( 'NONE',  ( 12.84374999795161543, -4.648860486681943627, -1.510506337161893642 ) ) ;
#408 = EDGE_CURVE ( 'NONE', #12256, #1337, #17055, .T. ) ;
#409 = DIRECTION ( 'NONE',  ( -1.000000000000000000, -0.000000000000000000, -0.000000000000000000 ) ) ;
#410 = CIRCLE ( 'NONE', #17678, 5.400000000000000355 ) ;
#411 = VERTEX_POINT ( 'NONE', #14043 ) ;
#412 = CIRCLE ( 'NONE', #11553, 1.000000000000004441 ) ;
#413 = ADVANCED_FACE ( 'NONE', ( #6417 ), #18643, .T. ) ;
#414 = STYLED_ITEM ( 'NONE', ( #11361 ), #2965 ) ;
#415 = CARTESIAN_POINT ( 'NONE',  ( -1.899999999999999023, 8.279592079675421725E-16, 6.760799999999997034 ) ) ;
#416 = CARTESIAN_POINT ( 'NONE',  ( 7.312499995903225525, 0.000000000000000000, -5.700000000000001066 ) ) ;
#417 = ORIENTED_EDGE ( 'NONE', *, *, #7596, .F. ) ;
#418 = PLANE ( 'NONE',  #2750 ) ;
#419 = CARTESIAN_POINT ( 'NONE',  ( 0.000000000000000000, -25.59481291497571220, -1.787276233276378314E-13 ) ) ;
#420 = ORIENTED_EDGE ( 'NONE', *, *, #3095, .T. ) ;
#421 = FACE_OUTER_BOUND ( 'NONE', #11319, .T. ) ;
#422 = ORIENTED_EDGE ( 'NONE', *, *, #14453, .F. ) ;
#423 = EDGE_CURVE ( 'NONE', #17227, #18545, #14802, .T. ) ;
#424 = CARTESIAN_POINT ( 'NONE',  ( -9.580134541264520465, -14.56230589874905235, -35.00000000000000000 ) ) ;
#425 = AXIS2_PLACEMENT_3D ( 'NONE', #7432, #4154, #17966 ) ;
#426 = B_SPLINE_CURVE_WITH_KNOTS ( 'NONE', 3,
 ( #7792, #796, #17497, #14401, #5671, #2568 ),
 .UNSPECIFIED., .F., .F.,
 ( 4, 2, 4 ),
 ( 0.008176170726434979844, 0.01049421029328160074, 0.01281224986012821990 ),
 .UNSPECIFIED. ) ;
#427 = ORIENTED_EDGE ( 'NONE', *, *, #9117, .T. ) ;
#428 = B_SPLINE_CURVE_WITH_KNOTS ( 'NONE', 3,
 ( #14907, #7276, #7374, #13499, #10410, #7684 ),
 .UNSPECIFIED., .F., .F.,
 ( 4, 2, 4 ),
 ( 2.132675795043207789E-07, 0.001878604073277004988, 0.003756994878974505639 ),
 .UNSPECIFIED. ) ;
#429 = EDGE_CURVE ( 'NONE', #1337, #18773, #8416, .T. ) ;
#430 = CARTESIAN_POINT ( 'NONE',  ( 17.68117051311639898, -3.372863662543048591, -32.00000000000000000 ) ) ;
#431 = CARTESIAN_POINT ( 'NONE',  ( 4.447186883680864788, 3.231070400981779667, -14.11718749948790830 ) ) ;
#432 = DIRECTION ( 'NONE',  ( 0.000000000000000000, 0.000000000000000000, 1.000000000000000000 ) ) ;
#433 = CIRCLE ( 'NONE', #15125, 24.12539914357697413 ) ;
#434 = CARTESIAN_POINT ( 'NONE',  ( 4.620319390059819398, -1.773574444220757274, -10.96874999795161720 ) ) ;
#435 = ORIENTED_EDGE ( 'NONE', *, *, #17905, .F. ) ;
#436 = B_SPLINE_CURVE_WITH_KNOTS ( 'NONE', 3,
 ( #7801, #2, #10814, #16923, #1712, #13914 ),
 .UNSPECIFIED., .F., .F.,
 ( 4, 2, 4 ),
 ( 2.586195665735896780E-07, 0.001878649493629692057, 0.003757040367692810780 ),
 .UNSPECIFIED. ) ;
#437 = VECTOR ( 'NONE', #17794, 1000.000000000000000 ) ;
#438 = PLANE ( 'NONE',  #10003 ) ;
#439 = DIRECTION ( 'NONE',  ( -1.000000000000000000, -0.000000000000000000, -0.000000000000000000 ) ) ;
#440 = EDGE_LOOP ( 'NONE', ( #15883, #17623 ) ) ;
#441 = PRESENTATION_LAYER_ASSIGNMENT (  '', '', ( #17051 ) ) ;
#442 = CARTESIAN_POINT ( 'NONE',  ( -6.929096493834647319, 2.870125742738179664, 12.00000000000000000 ) ) ;
#443 = EDGE_CURVE ( 'NONE', #4220, #16711, #7630, .T. ) ;
#444 = CARTESIAN_POINT ( 'NONE',  ( -1.799999999999999600, 9.797174393178827630E-16, 8.000000000000000000 ) ) ;
#445 = LINE ( 'NONE', #1934, #5840 ) ;
#446 = ORIENTED_EDGE ( 'NONE', *, *, #14016, .F. ) ;
#447 = CARTESIAN_POINT ( 'NONE',  ( 0.02436607992776628623, 24.63872515616082737, -2.336989772644355590 ) ) ;
#448 = CARTESIAN_POINT ( 'NONE',  ( 10.31249999590322552, -0.5958122406255588199, -5.668774803599165857 ) ) ;
#449 = VECTOR ( 'NONE', #17519, 1000.000000000000227 ) ;
#450 = ORIENTED_EDGE ( 'NONE', *, *, #18835, .T. ) ;
#451 = SHAPE_REPRESENTATION ( 'short pitch roller chain wheel_s_iso_Chain wheel ISO - 20Z 05B-1 --20SA8.0N', ( #16724 ), #120 ) ;
#452 = DIRECTION ( 'NONE',  ( 0.000000000000000000, 1.000000000000000000, 0.000000000000000000 ) ) ;
#453 = EDGE_CURVE ( 'NONE', #4439, #253, #13521, .T. ) ;
#454 = ORIENTED_EDGE ( 'NONE', *, *, #8309, .T. ) ;
#455 = APPLICATION_PROTOCOL_DEFINITION ( 'draft international standard', 'automotive_design', 1998, #1638 ) ;
#456 = EDGE_CURVE ( 'NONE', #15001, #196, #433, .T. ) ;
#457 = FILL_AREA_STYLE_COLOUR ( '', #2219 ) ;
#458 = ORIENTED_EDGE ( 'NONE', *, *, #3289, .T. ) ;
#459 = ORIENTED_EDGE ( 'NONE', *, *, #7878, .F. ) ;
#460 = CARTESIAN_POINT ( 'NONE',  ( 2.789999999999999147, 24.34211360614300190, 7.909232158574900140 ) ) ;
#461 =( GEOMETRIC_REPRESENTATION_CONTEXT ( 3 ) GLOBAL_UNCERTAINTY_ASSIGNED_CONTEXT ( ( #5578 ) ) GLOBAL_UNIT_ASSIGNED_CONTEXT ( ( #6065, #13682, #1180 ) ) REPRESENTATION_CONTEXT ( 'NONE', 'WORKASPACE' ) );
#462 = AXIS2_PLACEMENT_3D ( 'NONE', #16439, #9027, #7204 ) ;
#463 = CARTESIAN_POINT ( 'NONE',  ( 8.968749997951613651, 1.280903732194420996, 4.780397808154265960 ) ) ;
#464 = ORIENTED_EDGE ( 'NONE', *, *, #491, .T. ) ;
#465 = EDGE_CURVE ( 'NONE', #9137, #16676, #4084, .T. ) ;
#466 = FACE_BOUND ( 'NONE', #15200, .T. ) ;
#467 = AXIS2_PLACEMENT_3D ( 'NONE', #2237, #17453, #19046 ) ;
#468 = ORIENTED_EDGE ( 'NONE', *, *, #6736, .T. ) ;
#469 = AXIS2_PLACEMENT_3D ( 'NONE', #3938, #11542, #11357 ) ;
#470 = PLANE ( 'NONE',  #17230 ) ;
#471 = B_SPLINE_CURVE_WITH_KNOTS ( 'NONE', 3,
 ( #16379, #8875, #2659, #8775 ),
 .UNSPECIFIED., .F., .F.,
 ( 4, 4 ),
 ( 0.005258214619651984008, 0.005948481662034168192 ),
 .UNSPECIFIED. ) ;
#472 = CARTESIAN_POINT ( 'NONE',  ( 0.000000000000000000, 20.62201879784911540, 12.52067188844362100 ) ) ;
#473 = DIRECTION ( 'NONE',  ( 0.000000000000000000, 0.000000000000000000, -1.000000000000000000 ) ) ;
#474 = ORIENTED_EDGE ( 'NONE', *, *, #11666, .T. ) ;
#475 = DIRECTION ( 'NONE',  ( -0.000000000000000000, -0.000000000000000000, -1.000000000000000000 ) ) ;
#476 = ADVANCED_FACE ( 'NONE', ( #8445 ), #15472, .T. ) ;
#477 = AXIS2_PLACEMENT_3D ( 'NONE', #18214, #19704, #4602 ) ;
#478 = ORIENTED_EDGE ( 'NONE', *, *, #16286, .F. ) ;
#479 = VERTEX_POINT ( 'NONE', #7106 ) ;
#480 = CARTESIAN_POINT ( 'NONE',  ( -3.143139765844555900, 4.840010801796527318, -12.50000000000000533 ) ) ;
#481 = LINE ( 'NONE', #7970, #4863 ) ;
#482 = VECTOR ( 'NONE', #13106, 1000.000000000000000 ) ;
#483 = DIRECTION ( 'NONE',  ( -1.000000000000000000, -6.419766481290786633E-33, 0.000000000000000000 ) ) ;
#484 = ORIENTED_EDGE ( 'NONE', *, *, #3994, .T. ) ;
#485 = CARTESIAN_POINT ( 'NONE',  ( 12.46874999795161543, 3.632567103900569361, -3.270778111535288080 ) ) ;
#486 = B_SPLINE_CURVE_WITH_KNOTS ( 'NONE', 3,
 ( #997, #905, #15546, #3338 ),
 .UNSPECIFIED., .F., .F.,
 ( 4, 4 ),
 ( 2.324263106257895883E-07, 0.0006888201370294903293 ),
 .UNSPECIFIED. ) ;
#487 = DIRECTION ( 'NONE',  ( 0.000000000000000000, 1.000000000000000000, -1.224646799147353207E-16 ) ) ;
#488 = VERTEX_POINT ( 'NONE', #13041 ) ;
#489 = DIRECTION ( 'NONE',  ( 0.8660254037844380415, -0.5000000000000009992, 0.000000000000000000 ) ) ;
#490 = ADVANCED_FACE ( 'NONE', ( #16238 ), #3832, .F. ) ;
#491 = EDGE_CURVE ( 'NONE', #14026, #12070, #7010, .T. ) ;
#492 = ADVANCED_FACE ( 'NONE', ( #12129 ), #16089, .T. ) ;
#493 = DIRECTION ( 'NONE',  ( -1.000000000000000000, -0.000000000000000000, -0.000000000000000000 ) ) ;
#494 = DIRECTION ( 'NONE',  ( 0.000000000000000000, 0.7315216790650493905, -0.6818181818181815457 ) ) ;
#495 = CARTESIAN_POINT ( 'NONE',  ( 0.7592463941534238758, 3.797885586973211325, 27.31305418910211458 ) ) ;
#496 = CARTESIAN_POINT ( 'NONE',  ( 6.843749997951615427, 4.233219804643887585, -2.444050593749990785 ) ) ;
#497 = ORIENTED_EDGE ( 'NONE', *, *, #6656, .F. ) ;
#498 = CIRCLE ( 'NONE', #11670, 0.9999999999999974465 ) ;
#499 = DIRECTION ( 'NONE',  ( 1.000000000000000000, 0.000000000000000000, 0.000000000000000000 ) ) ;
#500 = SURFACE_SIDE_STYLE ('',( #17201 ) ) ;
#501 = TOROIDAL_SURFACE ( 'NONE', #12593, 8.800000000000022027, 0.1999999999999994282 ) ;
#502 = DIRECTION ( 'NONE',  ( -0.000000000000000000, -0.000000000000000000, 1.000000000000000000 ) ) ;
#503 = EDGE_CURVE ( 'NONE', #12346, #5672, #2341, .T. ) ;
#504 = EDGE_CURVE ( 'NONE', #17943, #9399, #4719, .T. ) ;
#505 = DIRECTION ( 'NONE',  ( 1.000000000000000000, 0.000000000000000000, 0.000000000000000000 ) ) ;
#506 = ORIENTED_EDGE ( 'NONE', *, *, #18779, .F. ) ;
#507 = CARTESIAN_POINT ( 'NONE',  ( 2.783025325906567371, -24.42374957165203853, -2.249040938978752013 ) ) ;
#508 = CARTESIAN_POINT ( 'NONE',  ( 2.789999999999999147, -5.535312321042557215, -23.48180575137735815 ) ) ;
#509 = CARTESIAN_POINT ( 'NONE',  ( 14.46874999795161720, -1.988169868018592856, 4.465502636338025688 ) ) ;
#510 = DIRECTION ( 'NONE',  ( 0.000000000000000000, 0.000000000000000000, 1.000000000000000000 ) ) ;
#511 = CARTESIAN_POINT ( 'NONE',  ( 0.000000000000000000, 0.000000000000000000, -30.00000000000000355 ) ) ;
#512 = ORIENTED_EDGE ( 'NONE', *, *, #15204, .T. ) ;
#513 = CARTESIAN_POINT ( 'NONE',  ( 5.668774803599156975, -0.5958122406256373127, -14.31249999590322552 ) ) ;
#514 = APPLICATION_CONTEXT ( 'automotive_design' ) ;
#515 = DIRECTION ( 'NONE',  ( 1.000000000000000000, 0.000000000000000000, -0.000000000000000000 ) ) ;
#516 = ORIENTED_EDGE ( 'NONE', *, *, #190, .T. ) ;
#517 = DIRECTION ( 'NONE',  ( 0.000000000000000000, 0.000000000000000000, -1.000000000000000000 ) ) ;
#518 = FACE_OUTER_BOUND ( 'NONE', #1664, .T. ) ;
#519 = AXIS2_PLACEMENT_3D ( 'NONE', #1734, #18343, #15443 ) ;
#520 = ORIENTED_EDGE ( 'NONE', *, *, #17895, .F. ) ;
#521 = CARTESIAN_POINT ( 'NONE',  ( -12.86923836996420611, -11.47363181547641275, 35.00000000000000000 ) ) ;
#522 = DIRECTION ( 'NONE',  ( -1.000000000000000000, -0.000000000000000000, -0.000000000000000000 ) ) ;
#523 = ORIENTED_EDGE ( 'NONE', *, *, #4370, .F. ) ;
#524 = CARTESIAN_POINT ( 'NONE',  ( -17.96448111170888851, 1.130229351527647585, 32.00000000000000000 ) ) ;
#525 = DIRECTION ( 'NONE',  ( -1.000000000000000000, 0.000000000000000000, 0.000000000000000000 ) ) ;
#526 = DIRECTION ( 'NONE',  ( 0.000000000000000000, 0.000000000000000000, 1.000000000000000000 ) ) ;
#527 = EDGE_CURVE ( 'NONE', #16516, #11599, #15232, .T. ) ;
#528 = EDGE_LOOP ( 'NONE', ( #18613, #17354, #7427, #17792, #19667, #11057 ) ) ;
#529 = CARTESIAN_POINT ( 'NONE',  ( -9.000000000000001776, 0.000000000000000000, -22.00000000000000000 ) ) ;
#530 = VERTEX_POINT ( 'NONE', #15333 ) ;
#531 = EDGE_CURVE ( 'NONE', #12054, #4447, #7429, .T. ) ;
#532 = CARTESIAN_POINT ( 'NONE',  ( 5.700000000000001954, -0.5990941410143687529, -10.98069898359950258 ) ) ;
#533 = AXIS2_PLACEMENT_3D ( 'NONE', #9932, #13023, #14624 ) ;
#534 = EDGE_LOOP ( 'NONE', ( #18812, #9374, #9796, #10381, #12618, #14253, #16988, #12583 ) ) ;
#535 = DIRECTION ( 'NONE',  ( 1.000000000000000000, 0.000000000000000000, 0.000000000000000000 ) ) ;
#536 = CIRCLE ( 'NONE', #18400, 0.03079999999999836341 ) ;
#537 = CARTESIAN_POINT ( 'NONE',  ( -4.942249507334558700, -0.2590123213420631454, -13.34374999795161365 ) ) ;
#538 = CARTESIAN_POINT ( 'NONE',  ( 12.32184790671639618, 13.12143529358541016, 32.00000000000000000 ) ) ;
#539 = CARTESIAN_POINT ( 'NONE',  ( 0.5279272933715194460, 19.66369668717032937, 18.56460150496945971 ) ) ;
#540 = VERTEX_POINT ( 'NONE', #1616 ) ;
#541 = CARTESIAN_POINT ( 'NONE',  ( 0.000000000000000000, 0.000000000000000000, -33.00000000000000000 ) ) ;
#542 = EDGE_CURVE ( 'NONE', #1723, #7592, #12575, .T. ) ;
#543 = CARTESIAN_POINT ( 'NONE',  ( 1.749999999999998002, 0.000000000000000000, 0.000000000000000000 ) ) ;
#544 = EDGE_LOOP ( 'NONE', ( #8721, #12859, #15196, #3818, #16637 ) ) ;
#545 = VECTOR ( 'NONE', #19579, 1000.000000000000000 ) ;
#546 = DIRECTION ( 'NONE',  ( -1.000000000000000000, -0.000000000000000000, -0.000000000000000000 ) ) ;
#547 = EDGE_CURVE ( 'NONE', #307, #4366, #2908, .T. ) ;
#548 = CIRCLE ( 'NONE', #12037, 4.000000000000000000 ) ;
#549 = B_SPLINE_CURVE_WITH_KNOTS ( 'NONE', 3,
 ( #17300, #8294, #9715, #15905 ),
 .UNSPECIFIED., .F., .F.,
 ( 4, 4 ),
 ( 3.059063720746924101E-07, 0.0006888942284913933487 ),
 .UNSPECIFIED. ) ;
#550 = LINE ( 'NONE', #6821, #5143 ) ;
#551 = CARTESIAN_POINT ( 'NONE',  ( 0.02436607992776281678, 2.336989772644269436, 24.63872515616083447 ) ) ;
#552 = ORIENTED_EDGE ( 'NONE', *, *, #14437, .T. ) ;
#553 = CARTESIAN_POINT ( 'NONE',  ( 2.789999999999999147, -16.37294372382871188, 18.55949924794887096 ) ) ;
#554 = CARTESIAN_POINT ( 'NONE',  ( 11.84374999795161365, 2.444050593750049405, -4.233219804643852946 ) ) ;
#555 = CARTESIAN_POINT ( 'NONE',  ( 9.343749997951615427, 1.280903732194420996, 4.780397808154265960 ) ) ;
#556 = ORIENTED_EDGE ( 'NONE', *, *, #11604, .T. ) ;
#557 = CARTESIAN_POINT ( 'NONE',  ( -12.00000000000000178, 0.000000000000000000, 35.00000000000000000 ) ) ;
#558 = ORIENTED_EDGE ( 'NONE', *, *, #6224, .F. ) ;
#559 = FACE_BOUND ( 'NONE', #1659, .T. ) ;
#560 = FACE_OUTER_BOUND ( 'NONE', #8813, .T. ) ;
#561 = EDGE_LOOP ( 'NONE', ( #1766, #13669, #6712, #18454, #1075, #7563, #16391, #5040 ) ) ;
#562 = VERTEX_POINT ( 'NONE', #12229 ) ;
#563 = DIRECTION ( 'NONE',  ( -0.000000000000000000, -0.000000000000000000, 1.000000000000000000 ) ) ;
#564 = CARTESIAN_POINT ( 'NONE',  ( 9.165444847914525184, 0.2987243419133224775, 5.700000000000001954 ) ) ;
#565 = VECTOR ( 'NONE', #8267, 1000.000000000000000 ) ;
#566 = CARTESIAN_POINT ( 'NONE',  ( 9.968749997951615427, -0.2590123213421313686, 4.942249507334556036 ) ) ;
#567 = CIRCLE ( 'NONE', #11727, 14.00000000000000178 ) ;
#568 = ORIENTED_EDGE ( 'NONE', *, *, #14160, .F. ) ;
#569 = VERTEX_POINT ( 'NONE', #18234 ) ;
#570 = CIRCLE ( 'NONE', #12063, 2.524999999999995914 ) ;
#571 = CARTESIAN_POINT ( 'NONE',  ( -2.318398865532109721, -5.207209108562803834, -9.000000000000005329 ) ) ;
#572 = AXIS2_PLACEMENT_3D ( 'NONE', #18958, #5144, #9567 ) ;
#573 = DIRECTION ( 'NONE',  ( 1.000000000000000000, 6.419766481290786633E-33, -0.000000000000000000 ) ) ;
#574 = FACE_BOUND ( 'NONE', #7715, .T. ) ;
#575 = ORIENTED_EDGE ( 'NONE', *, *, #10908, .T. ) ;
#576 = CYLINDRICAL_SURFACE ( 'NONE', #10772, 4.824999999999999289 ) ;
#577 = CYLINDRICAL_SURFACE ( 'NONE', #2328, 13.19999999999999929 ) ;
#578 = ORIENTED_EDGE ( 'NONE', *, *, #10615, .F. ) ;
#579 = ORIENTED_EDGE ( 'NONE', *, *, #19561, .F. ) ;
#580 = CARTESIAN_POINT ( 'NONE',  ( 5.000000000000000000, 1.999999999999998224, 37.99999999999999289 ) ) ;
#581 = B_SPLINE_CURVE_WITH_KNOTS ( 'NONE', 3,
 ( #3144, #12451, #4841, #13951, #18645, #4946 ),
 .UNSPECIFIED., .F., .F.,
 ( 4, 2, 4 ),
 ( 4.462636882221166670E-07, 0.001879885203074807814, 0.003759324142461393462 ),
 .UNSPECIFIED. ) ;
#582 = CARTESIAN_POINT ( 'NONE',  ( -2.000000000000001776, 3.950217066951266176, 3.681818181818181213 ) ) ;
#583 = AXIS2_PLACEMENT_3D ( 'NONE', #18408, #5087, #17013 ) ;
#584 = DIRECTION ( 'NONE',  ( 0.000000000000000000, 0.000000000000000000, -1.000000000000000000 ) ) ;
#585 = VECTOR ( 'NONE', #11111, 1000.000000000000000 ) ;
#586 = ORIENTED_EDGE ( 'NONE', *, *, #6888, .T. ) ;
#587 = CARTESIAN_POINT ( 'NONE',  ( -8.671566133830875600, 15.77352024078954429, -35.00000000000000000 ) ) ;
#588 = DIRECTION ( 'NONE',  ( -1.000000000000000000, -0.000000000000000000, -0.000000000000000000 ) ) ;
#589 = ORIENTED_EDGE ( 'NONE', *, *, #13563, .F. ) ;
#590 = FACE_OUTER_BOUND ( 'NONE', #15857, .T. ) ;
#591 = EDGE_CURVE ( 'NONE', #11430, #2770, #11411, .T. ) ;
#592 = CYLINDRICAL_SURFACE ( 'NONE', #9309, 28.06981291497571362 ) ;
#593 = CARTESIAN_POINT ( 'NONE',  ( 6.656249997951614539, 4.233219804643887585, -2.444050593749990341 ) ) ;
#594 = CARTESIAN_POINT ( 'NONE',  ( 0.000000000000000000, 0.000000000000000000, 12.00000000000000000 ) ) ;
#595 = CARTESIAN_POINT ( 'NONE',  ( -1.510506337161893642, -4.648860486681943627, -12.46874999795161543 ) ) ;
#596 = CIRCLE ( 'NONE', #10178, 3.000000000000000000 ) ;
#597 = CYLINDRICAL_SURFACE ( 'NONE', #3082, 1.000000000000004441 ) ;
#598 = CARTESIAN_POINT ( 'NONE',  ( 0.000000000000000000, 0.000000000000000000, -28.99999999999999645 ) ) ;
#599 = CARTESIAN_POINT ( 'NONE',  ( 0.2436698586202201144, 0.000000000000000000, 0.000000000000000000 ) ) ;
#600 = VERTEX_POINT ( 'NONE', #1222 ) ;
#601 = CYLINDRICAL_SURFACE ( 'NONE', #13048, 1.000000000000000888 ) ;
#602 = CARTESIAN_POINT ( 'NONE',  ( -39.64101615137757761, -1.650388831904890594E-13, 37.99999999999999289 ) ) ;
#603 = UNCERTAINTY_MEASURE_WITH_UNIT (LENGTH_MEASURE( 1.000000000000000082E-05 ), #7664, 'distance_accuracy_value', 'NONE');
#604 = CARTESIAN_POINT ( 'NONE',  ( 3.270778111535314281, -3.632567103900546712, -12.84374999795161543 ) ) ;
#605 = CARTESIAN_POINT ( 'NONE',  ( 0.000000000000000000, 22.25075486061737351, 9.324097380959511128 ) ) ;
#606 = CARTESIAN_POINT ( 'NONE',  ( 11.46874999795161543, -2.444050593749961031, -4.233219804643904460 ) ) ;
#607 = EDGE_CURVE ( 'NONE', #9627, #16718, #13871, .T. ) ;
#608 = VERTEX_POINT ( 'NONE', #10727 ) ;
#609 = DIRECTION ( 'NONE',  ( -1.000000000000000000, -0.000000000000000000, -0.000000000000000000 ) ) ;
#610 = ORIENTED_EDGE ( 'NONE', *, *, #19296, .F. ) ;
#611 = CARTESIAN_POINT ( 'NONE',  ( 11.50000000000000355, 3.631840208645857437, -4.484949146646330931 ) ) ;
#612 = CARTESIAN_POINT ( 'NONE',  ( -12.32184790671639085, 13.12143529358541549, -32.00000000000000000 ) ) ;
#613 = AXIS2_PLACEMENT_3D ( 'NONE', #10764, #563, #14261 ) ;
#614 = ORIENTED_EDGE ( 'NONE', *, *, #4205, .T. ) ;
#615 = EDGE_CURVE ( 'NONE', #13431, #17330, #7505, .T. ) ;
#616 = AXIS2_PLACEMENT_3D ( 'NONE', #5944, #11761, #47 ) ;
#617 = DIRECTION ( 'NONE',  ( 1.000000000000000000, 6.419766481290786633E-33, -0.000000000000000000 ) ) ;
#618 = CARTESIAN_POINT ( 'NONE',  ( 11.31249999590322375, 5.421022142882375938, -1.761396867937200739 ) ) ;
#619 = VERTEX_POINT ( 'NONE', #10824 ) ;
#620 = CARTESIAN_POINT ( 'NONE',  ( -6.626241948324210540, -16.73597674598852336, -32.00000000000000000 ) ) ;
#621 = CARTESIAN_POINT ( 'NONE',  ( 2.789999999999999147, 24.04302995059966364, 1.991882183130384121 ) ) ;
#622 = CARTESIAN_POINT ( 'NONE',  ( 0.000000000000000000, 0.000000000000000000, -33.00000000000000000 ) ) ;
#623 = ORIENTED_EDGE ( 'NONE', *, *, #8596, .T. ) ;
#624 = CARTESIAN_POINT ( 'NONE',  ( 6.968749997951614539, -0.7741991708319229115, 4.888101187499994893 ) ) ;
#625 = ORIENTED_EDGE ( 'NONE', *, *, #10006, .T. ) ;
#627 = DIRECTION ( 'NONE',  ( -1.000000000000000000, 0.000000000000000000, 0.000000000000000000 ) ) ;
#626 = VECTOR ( 'NONE', #14370, 1000.000000000000000 ) ;
#628 = ORIENTED_EDGE ( 'NONE', *, *, #19583, .T. ) ;
#629 = FACE_BOUND ( 'NONE', #5913, .T. ) ;
#630 = CARTESIAN_POINT ( 'NONE',  ( 0.5321745379877897975, 12.96514671151801323, -23.74442027961346113 ) ) ;
#631 = EDGE_CURVE ( 'NONE', #9247, #8012, #19426, .T. ) ;
#632 = CARTESIAN_POINT ( 'NONE',  ( 0.000000000000000000, -22.25075486061745167, 9.324097380959385006 ) ) ;
#633 = AXIS2_PLACEMENT_3D ( 'NONE', #11254, #17358, #4851 ) ;
#634 = CARTESIAN_POINT ( 'NONE',  ( 3.632567103900546712, 3.270778111535313837, -7.843749997951614539 ) ) ;
#635 = EDGE_LOOP ( 'NONE', ( #13880, #12061, #1911, #8139 ) ) ;
#636 = FACE_BOUND ( 'NONE', #2747, .T. ) ;
#637 = DIRECTION ( 'NONE',  ( 0.000000000000000000, 0.000000000000000000, 1.000000000000000000 ) ) ;
#638 = ADVANCED_FACE ( 'NONE', ( #7400 ), #13014, .T. ) ;
#639 = VERTEX_POINT ( 'NONE', #10529 ) ;
#640 = ADVANCED_FACE ( 'NONE', ( #14022 ), #1910, .T. ) ;
#641 = CARTESIAN_POINT ( 'NONE',  ( 1.800000000000000044, 0.000000000000000000, 0.000000000000000000 ) ) ;
#642 = LINE ( 'NONE', #1837, #19205 ) ;
#643 = CARTESIAN_POINT ( 'NONE',  ( 0.02436607992776585255, -5.391175441198789109, 24.15498966839961170 ) ) ;
#644 = ORIENTED_EDGE ( 'NONE', *, *, #6204, .T. ) ;
#646 = FACE_OUTER_BOUND ( 'NONE', #17475, .T. ) ;
#645 = CIRCLE ( 'NONE', #13735, 5.700000000000002842 ) ;
#647 = CARTESIAN_POINT ( 'NONE',  ( 2.246813503491803310, -4.409619785863921670, -9.968749997951615427 ) ) ;
#648 = CARTESIAN_POINT ( 'NONE',  ( -39.64101615137763446, 12.80384757729311573, 37.99999999999999289 ) ) ;
#649 = EDGE_LOOP ( 'NONE', ( #15973, #2519, #13118, #2689 ) ) ;
#650 = EDGE_CURVE ( 'NONE', #1292, #12256, #16241, .T. ) ;
#651 = FACE_OUTER_BOUND ( 'NONE', #5044, .T. ) ;
#652 = EDGE_LOOP ( 'NONE', ( #11686, #13562, #787, #7989 ) ) ;
#653 = CARTESIAN_POINT ( 'NONE',  ( 8.843749997951615427, 1.988169868018562436, 4.465502636338039011 ) ) ;
#654 = CARTESIAN_POINT ( 'NONE',  ( 14.46874999795161720, -1.988169868018592856, 4.465502636338025688 ) ) ;
#655 = ORIENTED_EDGE ( 'NONE', *, *, #19266, .F. ) ;
#656 = EDGE_LOOP ( 'NONE', ( #12086, #15329 ) ) ;
#657 = CARTESIAN_POINT ( 'NONE',  ( 7.288264926088301010, -4.957553806382933637, -0.4925372136696608560 ) ) ;
#658 = DIRECTION ( 'NONE',  ( -1.000000000000000000, 0.000000000000000000, 0.000000000000000000 ) ) ;
#659 = CARTESIAN_POINT ( 'NONE',  ( 13.00000000000000000, -4.125339889944092953, 2.622041954598548941 ) ) ;
#660 = EDGE_CURVE ( 'NONE', #13507, #7007, #3581, .T. ) ;
#661 = ORIENTED_EDGE ( 'NONE', *, *, #17194, .F. ) ;
#662 = EDGE_CURVE ( 'NONE', #16700, #600, #4069, .T. ) ;
#663 = VECTOR ( 'NONE', #1603, 1000.000000000000000 ) ;
#664 = CIRCLE ( 'NONE', #18238, 5.700000000000001954 ) ;
#665 = CARTESIAN_POINT ( 'NONE',  ( 1.749999999999998002, 25.12109765559653596, 12.52377138324232675 ) ) ;
#666 = ORIENTED_EDGE ( 'NONE', *, *, #14685, .T. ) ;
#667 = EDGE_CURVE ( 'NONE', #62, #18274, #7812, .T. ) ;
#668 = CARTESIAN_POINT ( 'NONE',  ( 13.46874999795161543, 0.5109457054262118714, -4.861323657744403448 ) ) ;
#669 = ADVANCED_FACE ( 'NONE', ( #3317 ), #12722, .F. ) ;
#670 = DIRECTION ( 'NONE',  ( 0.000000000000000000, 0.000000000000000000, -1.000000000000000000 ) ) ;
#671 = CARTESIAN_POINT ( 'NONE',  ( 0.7592463977762113903, 27.14986936243574078, 4.828194074574446049 ) ) ;
#672 = ORIENTED_EDGE ( 'NONE', *, *, #13623, .F. ) ;
#673 = AXIS2_PLACEMENT_3D ( 'NONE', #19698, #12103, #2886 ) ;
#674 = LINE ( 'NONE', #2526, #7891 ) ;
#675 =( LENGTH_UNIT ( ) NAMED_UNIT ( * ) SI_UNIT ( .MILLI., .METRE. ) );
#676 = VERTEX_POINT ( 'NONE', #5011 ) ;
#677 = VERTEX_POINT ( 'NONE', #18521 ) ;
#678 = CARTESIAN_POINT ( 'NONE',  ( -1.493657965219446382, 5.574407415329178939, -13.50000000000000533 ) ) ;
#679 = ADVANCED_FACE ( 'NONE', ( #2109 ), #5546, .F. ) ;
#680 = CYLINDRICAL_SURFACE ( 'NONE', #3555, 2.524999999999995914 ) ;
#681 = DIRECTION ( 'NONE',  ( 1.000000000000000000, -0.000000000000000000, -0.000000000000000000 ) ) ;
#682 = EDGE_LOOP ( 'NONE', ( #3661, #6850, #15777, #2392 ) ) ;
#683 = CARTESIAN_POINT ( 'NONE',  ( 0.000000000000000000, -23.48180575137736170, 5.535312321042622052 ) ) ;
#684 =( BOUNDED_CURVE ( )  B_SPLINE_CURVE ( 2, ( #2775, #16596, #17896, #2575, #14700, #16400, #18096, #2876, #8691, #8990, #898, #990, #7068, #11693, #17798, #4094, #14800 ),
 .UNSPECIFIED., .F., .F. ) 
 B_SPLINE_CURVE_WITH_KNOTS ( ( 3, 2, 2, 2, 2, 2, 2, 2, 3 ),
 ( 0.000000000000000000, 0.05000000000000000971, 0.1000000000000000194, 0.1499999999999999944, 0.2000000000000000389, 0.2500000000000000000, 0.2999999999999999889, 0.3499999999999999223, 0.4000000000000000777 ),
 .UNSPECIFIED. ) 
 CURVE ( )  GEOMETRIC_REPRESENTATION_ITEM ( )  RATIONAL_B_SPLINE_CURVE ( ( 1.000000000000000000, 0.9876883405951377704, 1.000000000000000000, 0.9876883405951377704, 1.000000000000000000, 0.9876883405951377704, 1.000000000000000000, 0.9876883405951377704, 1.000000000000000000, 0.9876883405951377704, 1.000000000000000000, 0.9876883405951377704, 1.000000000000000000, 0.9876883405951377704, 1.000000000000000000, 0.9876883405951377704, 1.000000000000000000 ) ) 
 REPRESENTATION_ITEM ( '' )  );
#685 = CARTESIAN_POINT ( 'NONE',  ( 13.00000000000000178, -4.444590484536226960, -2.035510078342938733 ) ) ;
#686 = CIRCLE ( 'NONE', #9968, 8.239200000000002078 ) ;
#687 = ORIENTED_EDGE ( 'NONE', *, *, #13822, .F. ) ;
#688 = CARTESIAN_POINT ( 'NONE',  ( 2.765633920072239516, 16.37294372382858398, 18.55949924794898465 ) ) ;
#689 = CIRCLE ( 'NONE', #18568, 9.000000000000000000 ) ;
#690 = CARTESIAN_POINT ( 'NONE',  ( 2.000000000000000000, -2.000000000000002665, 37.99999999999999289 ) ) ;
#691 = CARTESIAN_POINT ( 'NONE',  ( 0.1855655959470677019, -19.17825124759764677, -17.45907811351477079 ) ) ;
#692 = LINE ( 'NONE', #10095, #9730 ) ;
#693 = CARTESIAN_POINT ( 'NONE',  ( 5.142044285764733935, -2.620002426024580000, -7.500000000000005329 ) ) ;
#694 = CARTESIAN_POINT ( 'NONE',  ( 1.394999999999999574, -27.68468304288262161, 4.633866840648820151 ) ) ;
#695 = PRESENTATION_STYLE_ASSIGNMENT (( #7886 ) ) ;
#696 = CARTESIAN_POINT ( 'NONE',  ( -2.000000000000001776, 0.000000000000000000, -6.735000000000022524 ) ) ;
#697 = DIRECTION ( 'NONE',  ( 0.000000000000000000, -1.000000000000000000, 0.000000000000000000 ) ) ;
#698 = ORIENTED_EDGE ( 'NONE', *, *, #15318, .F. ) ;
#699 = DIRECTION ( 'NONE',  ( 0.000000000000000000, 0.000000000000000000, 1.000000000000000000 ) ) ;
#700 = VECTOR ( 'NONE', #12818, 1000.000000000000000 ) ;
#701 = CARTESIAN_POINT ( 'NONE',  ( -2.299999999999996270, 0.000000000000000000, -6.000000000000020428 ) ) ;
#702 = DIRECTION ( 'NONE',  ( 6.419766481290786633E-33, -1.000000000000000000, 0.000000000000000000 ) ) ;
#703 = EDGE_CURVE ( 'NONE', #2779, #5327, #19540, .T. ) ;
#704 = FACE_OUTER_BOUND ( 'NONE', #6201, .T. ) ;
#705 = ORIENTED_EDGE ( 'NONE', *, *, #2287, .T. ) ;
#706 = LINE ( 'NONE', #3697, #393 ) ;
#707 = CARTESIAN_POINT ( 'NONE',  ( 3.954556930911861112, 2.873153789725825913, -14.84374999795161543 ) ) ;
#708 = ORIENTED_EDGE ( 'NONE', *, *, #12930, .T. ) ;
#709 = CARTESIAN_POINT ( 'NONE',  ( 2.789999999999999147, -23.31896751603337137, 7.334849878007427826 ) ) ;
#710 = PLANE ( 'NONE',  #13946 ) ;
#711 = ORIENTED_EDGE ( 'NONE', *, *, #7911, .F. ) ;
#712 = FACE_OUTER_BOUND ( 'NONE', #13492, .T. ) ;
#713 = EDGE_CURVE ( 'NONE', #18575, #7007, #1785, .T. ) ;
#714 = CARTESIAN_POINT ( 'NONE',  ( 2.030753602223783538, 4.828194074574346573, 27.14986936243576565 ) ) ;
#715 = CIRCLE ( 'NONE', #14455, 1.199999999999999734 ) ;
#716 = AXIS2_PLACEMENT_3D ( 'NONE', #3976, #1170, #14686 ) ;
#717 = CONICAL_SURFACE ( 'NONE', #10300, 3.593999999999999861, 0.2132412839022293782 ) ;
#718 = CARTESIAN_POINT ( 'NONE',  ( 9.671566133830877376, 15.77352024078954784, -32.00000000000000000 ) ) ;
#719 = DIRECTION ( 'NONE',  ( -1.000000000000000000, 0.000000000000000000, 0.000000000000000000 ) ) ;
#720 = VERTEX_POINT ( 'NONE', #3211 ) ;
#721 = DIRECTION ( 'NONE',  ( -1.000000000000000000, 0.000000000000000000, 0.000000000000000000 ) ) ;
#722 = FILL_AREA_STYLE_COLOUR ( '', #9371 ) ;
#723 = DIRECTION ( 'NONE',  ( 0.000000000000000000, 0.000000000000000000, -1.000000000000000000 ) ) ;
#724 = AXIS2_PLACEMENT_3D ( 'NONE', #2473, #11787, #4282 ) ;
#725 = VERTEX_POINT ( 'NONE', #9325 ) ;
#726 = DIRECTION ( 'NONE',  ( -1.000000000000000000, 0.000000000000000000, 0.000000000000000000 ) ) ;
#727 = ORIENTED_EDGE ( 'NONE', *, *, #2944, .F. ) ;
#728 = CARTESIAN_POINT ( 'NONE',  ( 2.765633920072239516, -2.336989772644097574, -24.63872515616085224 ) ) ;
#729 = ORIENTED_EDGE ( 'NONE', *, *, #5218, .T. ) ;
#730 = DIRECTION ( 'NONE',  ( 0.000000000000000000, -1.000000000000000000, 0.000000000000000000 ) ) ;
#731 = EDGE_CURVE ( 'NONE', #4617, #19646, #9712, .T. ) ;
#732 = CARTESIAN_POINT ( 'NONE',  ( 4.611396867937200383, 3.350375938067097881, -15.31249999590322552 ) ) ;
#733 = DIRECTION ( 'NONE',  ( 0.000000000000000000, 0.000000000000000000, -1.000000000000000000 ) ) ;
#734 = TOROIDAL_SURFACE ( 'NONE', #17664, 24.12539914357697413, 8.000000000000000000 ) ;
#735 = DIRECTION ( 'NONE',  ( 1.000000000000000000, 0.000000000000000000, 0.000000000000000000 ) ) ;
#736 = VERTEX_POINT ( 'NONE', #10923 ) ;
#737 = AXIS2_PLACEMENT_3D ( 'NONE', #19098, #609, #6683 ) ;
#738 = FACE_BOUND ( 'NONE', #4707, .T. ) ;
#739 = CARTESIAN_POINT ( 'NONE',  ( 2.789999999999999147, -22.71065055754459650, 9.836394144775621129 ) ) ;
#740 = ORIENTED_EDGE ( 'NONE', *, *, #3539, .T. ) ;
#741 = AXIS2_PLACEMENT_3D ( 'NONE', #12660, #7645, #17254 ) ;
#742 = CARTESIAN_POINT ( 'NONE',  ( -11.58013454126452579, -14.56230589874905235, -32.00000000000000000 ) ) ;
#743 = DIRECTION ( 'NONE',  ( 0.000000000000000000, 0.000000000000000000, -1.000000000000000000 ) ) ;
#744 = EDGE_CURVE ( 'NONE', #18193, #12621, #16104, .T. ) ;
#745 = CARTESIAN_POINT ( 'NONE',  ( 5.421022142882364392, -1.761396867937238486, -8.312499995903225525 ) ) ;
#746 = ADVANCED_FACE ( 'NONE', ( #7179 ), #9075, .T. ) ;
#747 = ORIENTED_EDGE ( 'NONE', *, *, #8475, .F. ) ;
#748 = CARTESIAN_POINT ( 'NONE',  ( -7.937500000000000000, -1.543790678740078581, -0.06656457167770332695 ) ) ;
#749 = DIRECTION ( 'NONE',  ( 1.000000000000000000, 0.000000000000000000, 0.000000000000000000 ) ) ;
#750 = VERTEX_POINT ( 'NONE', #5499 ) ;
#751 = CARTESIAN_POINT ( 'NONE',  ( 1.039999999999996039, 19.67366047555559305, -20.02152543075323976 ) ) ;
#752 = ORIENTED_EDGE ( 'NONE', *, *, #660, .F. ) ;
#753 = AXIS2_PLACEMENT_3D ( 'NONE', #9858, #9653, #15648 ) ;
#754 = CARTESIAN_POINT ( 'NONE',  ( 13.00000000000000178, -4.920309236097862637, -1.604440756441545268 ) ) ;
#755 = FACE_OUTER_BOUND ( 'NONE', #6243, .T. ) ;
#756 = VECTOR ( 'NONE', #1088, 1000.000000000000000 ) ;
#757 = CARTESIAN_POINT ( 'NONE',  ( 0.000000000000000000, 0.000000000000000000, -28.99999999999999645 ) ) ;
#758 = VERTEX_POINT ( 'NONE', #14421 ) ;
#759 = VERTEX_POINT ( 'NONE', #16217 ) ;
#760 = B_SPLINE_CURVE_WITH_KNOTS ( 'NONE', 1,
 ( #6972, #5479 ),
 .UNSPECIFIED., .F., .F.,
 ( 2, 2 ),
 ( 0.000000000000000000, 1.000000000000000000 ),
 .UNSPECIFIED. ) ;
#761 = DIRECTION ( 'NONE',  ( -1.000000000000000000, -0.000000000000000000, -0.000000000000000000 ) ) ;
#762 = CARTESIAN_POINT ( 'NONE',  ( 12.65441706489329299, -5.699999999999998401, -0.6173595171471657483 ) ) ;
#763 = DIRECTION ( 'NONE',  ( 0.000000000000000000, -1.000000000000000000, 0.000000000000000000 ) ) ;
#764 = ORIENTED_EDGE ( 'NONE', *, *, #5632, .T. ) ;
#765 = MECHANICAL_DESIGN_GEOMETRIC_PRESENTATION_REPRESENTATION (  '', ( #9068 ), #11313 ) ;
#766 = SURFACE_STYLE_FILL_AREA ( #5055 ) ;
#767 = PRODUCT_DEFINITION_SHAPE ( 'NONE', 'NONE',  #9076 ) ;
#768 = VERTEX_POINT ( 'NONE', #1106 ) ;
#769 = VECTOR ( 'NONE', #719, 1000.000000000000000 ) ;
#770 = CARTESIAN_POINT ( 'NONE',  ( -18.96448111170889206, 1.130229351527647585, -35.00000000000000000 ) ) ;
#771 = DIRECTION ( 'NONE',  ( 0.000000000000000000, 0.000000000000000000, 1.000000000000000000 ) ) ;
#772 = CARTESIAN_POINT ( 'NONE',  ( -4.780397808154273953, -1.280903732194386579, -8.968749997951611874 ) ) ;
#773 = PRESENTATION_LAYER_ASSIGNMENT (  '', '', ( #16753 ) ) ;
#774 = EDGE_CURVE ( 'NONE', #12919, #10924, #14811, .T. ) ;
#775 = ORIENTED_EDGE ( 'NONE', *, *, #17901, .F. ) ;
#776 = EDGE_LOOP ( 'NONE', ( #15679, #8898, #8555, #10719 ) ) ;
#777 = EDGE_CURVE ( 'NONE', #2407, #17288, #6813, .T. ) ;
#778 = FACE_OUTER_BOUND ( 'NONE', #6078, .T. ) ;
#779 = CONICAL_SURFACE ( 'NONE', #10686, 3.323500000000020993, 0.7853981633974463916 ) ;
#780 = DIRECTION ( 'NONE',  ( 0.000000000000000000, 0.000000000000000000, 1.000000000000000000 ) ) ;
#781 = CARTESIAN_POINT ( 'NONE',  ( 12.66727757604273386, -4.360680574150373717E-16, 5.700000000000001066 ) ) ;
#782 = ORIENTED_EDGE ( 'NONE', *, *, #15988, .T. ) ;
#783 = EDGE_CURVE ( 'NONE', #14953, #18565, #5859, .T. ) ;
#784 = LINE ( 'NONE', #5274, #11574 ) ;
#785 = DIRECTION ( 'NONE',  ( -1.000000000000000000, -0.000000000000000000, -0.000000000000000000 ) ) ;
#786 = AXIS2_PLACEMENT_3D ( 'NONE', #14254, #7938, #12454 ) ;
#787 = ORIENTED_EDGE ( 'NONE', *, *, #9672, .F. ) ;
#788 = DIRECTION ( 'NONE',  ( 1.000000000000000000, 0.000000000000000000, -0.000000000000000000 ) ) ;
#789 = CARTESIAN_POINT ( 'NONE',  ( 1.749999999999998002, 0.000000000000000000, 0.000000000000000000 ) ) ;
#790 = EDGE_CURVE ( 'NONE', #17079, #15015, #15922, .T. ) ;
#791 = AXIS2_PLACEMENT_3D ( 'NONE', #5408, #8423, #8809 ) ;
#792 = DIRECTION ( 'NONE',  ( 0.000000000000000000, 0.000000000000000000, 1.000000000000000000 ) ) ;
#793 = DIRECTION ( 'NONE',  ( -1.000000000000000000, 0.000000000000000000, 0.000000000000000000 ) ) ;
#794 = CARTESIAN_POINT ( 'NONE',  ( 10.34374999795161543, -4.150607464521772094, -2.695436003842760719 ) ) ;
#795 = CARTESIAN_POINT ( 'NONE',  ( 9.312499995903225525, 2.318398865532038666, 5.207209108562838473 ) ) ;
#796 = CARTESIAN_POINT ( 'NONE',  ( 7.937499999999998224, -3.837375845242625871, -0.4937872269236130429 ) ) ;
#797 = CARTESIAN_POINT ( 'NONE',  ( -15.19790265903627180, 9.644882309621941374, 35.00000000000000000 ) ) ;
#798 = ORIENTED_EDGE ( 'NONE', *, *, #9859, .T. ) ;
#799 = CARTESIAN_POINT ( 'NONE',  ( -9.000000000000001776, 0.000000000000000000, -30.00000000000000355 ) ) ;
#800 = CIRCLE ( 'NONE', #3027, 6.500000000000002665 ) ;
#801 = CYLINDRICAL_SURFACE ( 'NONE', #8075, 8.000000000000000000 ) ;
#802 = UNCERTAINTY_MEASURE_WITH_UNIT (LENGTH_MEASURE( 1.000000000000000082E-05 ), #13780, 'distance_accuracy_value', 'NONE');
#803 = CARTESIAN_POINT ( 'NONE',  ( 1.493657965219485462, -5.574407415329169169, -14.81249999590322552 ) ) ;
#804 = CARTESIAN_POINT ( 'NONE',  ( 13.84374999795161543, 0.5109457054262118714, -4.861323657744403448 ) ) ;
#805 =( BOUNDED_SURFACE ( )  B_SPLINE_SURFACE ( 1, 2, ( 
 ( #16231, #11437, #17538, #3824, #17827, #9121, #4217, #4316, #13231, #11820, #13517, #19717, #19317, #10427, #6000, #15122, #10232 ),
 ( #4119, #11722, #1314, #10524, #14925, #17927, #8719, #5609, #2806, #16728, #14826, #16326, #16528, #5906, #13620, #3008, #12123 ) ),
 .UNSPECIFIED., .F., .F., .F. ) 
 B_SPLINE_SURFACE_WITH_KNOTS ( ( 2, 2 ),
 ( 3, 2, 2, 2, 2, 2, 2, 2, 3 ),
 ( 0.000000000000000000, 1.000000000000000000 ),
 ( 0.000000000000000000, 0.05000000000000000278, 0.1000000000000000056, 0.1499999999999999944, 0.2000000000000000111, 0.2500000000000000000, 0.2999999999999999889, 0.3499999999999999778, 0.4000000000000000222 ),
 .UNSPECIFIED. ) 
 GEOMETRIC_REPRESENTATION_ITEM ( )  RATIONAL_B_SPLINE_SURFACE ( (
 ( 1.000000000000000000, 0.9876883405951377704, 1.000000000000000000, 0.9876883405951377704, 1.000000000000000000, 0.9876883405951377704, 1.000000000000000000, 0.9876883405951377704, 1.000000000000000000, 0.9876883405951377704, 1.000000000000000000, 0.9876883405951377704, 1.000000000000000000, 0.9876883405951377704, 1.000000000000000000, 0.9876883405951377704, 1.000000000000000000),
 ( 1.000000000000000000, 0.9876883405951377704, 1.000000000000000000, 0.9876883405951377704, 1.000000000000000000, 0.9876883405951377704, 1.000000000000000000, 0.9876883405951377704, 1.000000000000000000, 0.9876883405951377704, 1.000000000000000000, 0.9876883405951377704, 1.000000000000000000, 0.9876883405951377704, 1.000000000000000000, 0.9876883405951377704, 1.000000000000000000) ) ) 
 REPRESENTATION_ITEM ( '' )  SURFACE ( )  );
#806 = DIRECTION ( 'NONE',  ( 0.000000000000000000, 0.000000000000000000, 1.000000000000000000 ) ) ;
#807 =( REPRESENTATION_RELATIONSHIP ('NONE','NONE', #18211, #12077 ) REPRESENTATION_RELATIONSHIP_WITH_TRANSFORMATION ( #17458 )SHAPE_REPRESENTATION_RELATIONSHIP( ) );
#808 = LINE ( 'NONE', #16007, #5368 ) ;
#809 = VERTEX_POINT ( 'NONE', #13215 ) ;
#810 = DIRECTION ( 'NONE',  ( -1.000000000000000000, 0.000000000000000000, 0.000000000000000000 ) ) ;
#811 = ADVANCED_FACE ( 'NONE', ( #819 ), #5404, .T. ) ;
#812 = CARTESIAN_POINT ( 'NONE',  ( 2.789999999999999147, 12.52067188844351442, 20.62201879784917935 ) ) ;
#813 = VERTEX_POINT ( 'NONE', #13020 ) ;
#814 = CARTESIAN_POINT ( 'NONE',  ( -90.00000000000000000, 0.000000000000000000, 0.000000000000000000 ) ) ;
#815 = DIRECTION ( 'NONE',  ( -1.000000000000000000, 0.000000000000000000, -0.000000000000000000 ) ) ;
#816 = EDGE_CURVE ( 'NONE', #10379, #5629, #19401, .T. ) ;
#817 = VECTOR ( 'NONE', #17686, 1000.000000000000000 ) ;
#818 = DIRECTION ( 'NONE',  ( 1.000000000000000000, 6.419766481290786633E-33, -0.000000000000000000 ) ) ;
#819 = FACE_OUTER_BOUND ( 'NONE', #16646, .T. ) ;
#820 = ORIENTED_EDGE ( 'NONE', *, *, #2202, .T. ) ;
#821 = DIRECTION ( 'NONE',  ( 1.000000000000000000, 0.000000000000000000, 0.000000000000000000 ) ) ;
#822 = PRESENTATION_STYLE_ASSIGNMENT (( #14625 ) ) ;
#823 = DIRECTION ( 'NONE',  ( 1.000000000000000000, 0.000000000000000000, 0.000000000000000000 ) ) ;
#824 = EDGE_LOOP ( 'NONE', ( #14773, #17764, #4685, #8934 ) ) ;
#825 = CARTESIAN_POINT ( 'NONE',  ( -2.000000000000001776, 0.000000000000000000, 0.000000000000000000 ) ) ;
#826 = ORIENTED_EDGE ( 'NONE', *, *, #7927, .F. ) ;
#827 = CARTESIAN_POINT ( 'NONE',  ( 8.776855558857221240, 3.635492607468361559, 0.000000000000000000 ) ) ;
#828 = ORIENTED_EDGE ( 'NONE', *, *, #12966, .F. ) ;
#829 = CARTESIAN_POINT ( 'NONE',  ( -16.28688694438836038, -7.664027248171298545, -32.00000000000000000 ) ) ;
#830 = FACE_OUTER_BOUND ( 'NONE', #14532, .T. ) ;
#831 = CYLINDRICAL_SURFACE ( 'NONE', #13469, 13.19999999999999929 ) ;
#832 = CIRCLE ( 'NONE', #13920, 8.265000000000021885 ) ;
#833 = DIRECTION ( 'NONE',  ( -0.000000000000000000, -0.000000000000000000, 1.000000000000000000 ) ) ;
#834 = AXIS2_PLACEMENT_3D ( 'NONE', #19075, #17680, #9988 ) ;
#835 = ORIENTED_EDGE ( 'NONE', *, *, #7451, .T. ) ;
#836 = B_SPLINE_CURVE_WITH_KNOTS ( 'NONE', 3,
 ( #844, #7013, #11538, #2423 ),
 .UNSPECIFIED., .F., .F.,
 ( 4, 4 ),
 ( 0.005258105385878707357, 0.005948373736081385803 ),
 .UNSPECIFIED. ) ;
#837 = FACE_BOUND ( 'NONE', #6605, .T. ) ;
#838 = EDGE_CURVE ( 'NONE', #8012, #12976, #9469, .T. ) ;
#839 = ORIENTED_EDGE ( 'NONE', *, *, #19666, .F. ) ;
#840 = EDGE_CURVE ( 'NONE', #6761, #4306, #6819, .T. ) ;
#841 = DIRECTION ( 'NONE',  ( -0.000000000000000000, -0.000000000000000000, 1.000000000000000000 ) ) ;
#842 = CARTESIAN_POINT ( 'NONE',  ( 1.510506337161829027, -4.648860486681964055, -10.84374999795161543 ) ) ;
#843 = ORIENTED_EDGE ( 'NONE', *, *, #491, .F. ) ;
#844 = CARTESIAN_POINT ( 'NONE',  ( 0.000000000000000000, 9.324097380959777581, -22.25075486061729535 ) ) ;
#845 = CARTESIAN_POINT ( 'NONE',  ( -90.00000000000000000, 1.102182119232620672E-15, 9.000000000000021316 ) ) ;
#846 = FACE_BOUND ( 'NONE', #14940, .T. ) ;
#847 = VECTOR ( 'NONE', #4218, 1000.000000000000000 ) ;
#848 = ORIENTED_EDGE ( 'NONE', *, *, #11223, .F. ) ;
#849 = CARTESIAN_POINT ( 'NONE',  ( 0.7592463977762105021, -27.14986936243570526, -4.828194074574642336 ) ) ;
#850 = ORIENTED_EDGE ( 'NONE', *, *, #16620, .T. ) ;
#851 = DIRECTION ( 'NONE',  ( 1.000000000000000000, 0.000000000000000000, 0.000000000000000000 ) ) ;
#852 = CYLINDRICAL_SURFACE ( 'NONE', #12511, 2.524999999999995914 ) ;
#853 = ORIENTED_EDGE ( 'NONE', *, *, #15946, .F. ) ;
#854 = CARTESIAN_POINT ( 'NONE',  ( -2.500000000000002220, 0.000000000000000000, 0.000000000000000000 ) ) ;
#855 = DIRECTION ( 'NONE',  ( 1.000000000000000000, 0.000000000000000000, 0.000000000000000000 ) ) ;
#856 = CARTESIAN_POINT ( 'NONE',  ( 2.000000000000000000, 1.999999999999998224, 37.99999999999999289 ) ) ;
#857 = ORIENTED_EDGE ( 'NONE', *, *, #17755, .F. ) ;
#858 = EDGE_CURVE ( 'NONE', #1292, #4347, #3906, .T. ) ;
#859 = AXIS2_PLACEMENT_3D ( 'NONE', #9005, #17910, #4106 ) ;
#860 = ORIENTED_EDGE ( 'NONE', *, *, #16548, .F. ) ;
#861 = EDGE_CURVE ( 'NONE', #6715, #196, #5862, .T. ) ;
#862 = DIRECTION ( 'NONE',  ( -1.000000000000000000, 0.000000000000000000, 0.000000000000000000 ) ) ;
#863 = CARTESIAN_POINT ( 'NONE',  ( 7.000000000000005329, -1.761396867937238486, 5.421022142882364392 ) ) ;
#864 = ORIENTED_EDGE ( 'NONE', *, *, #1510, .F. ) ;
#865 = DIRECTION ( 'NONE',  ( 0.000000000000000000, 0.000000000000000000, -1.000000000000000000 ) ) ;
#866 = VECTOR ( 'NONE', #8883, 1000.000000000000000 ) ;
#867 = DIRECTION ( 'NONE',  ( 0.8311608875373134309, -0.5560319946083909226, 0.000000000000000000 ) ) ;
#868 = CARTESIAN_POINT ( 'NONE',  ( 4.861323657744406113, -0.5109457054261780096, -13.46874999795161543 ) ) ;
#869 = AXIS2_PLACEMENT_3D ( 'NONE', #3599, #3403, #18508 ) ;
#870 = VERTEX_POINT ( 'NONE', #16016 ) ;
#871 = VERTEX_POINT ( 'NONE', #14621 ) ;
#872 = CARTESIAN_POINT ( 'NONE',  ( 2.789999999999999147, -9.514945144208585504, -22.37986894186682107 ) ) ;
#873 = EDGE_CURVE ( 'NONE', #3731, #5937, #2990, .T. ) ;
#874 = CARTESIAN_POINT ( 'NONE',  ( 2.718131885465892239, -16.91241718341984779, -18.89333555428573774 ) ) ;
#875 = CARTESIAN_POINT ( 'NONE',  ( -0.3020334839682475847, 5.763142191869157216, -7.500000000000005329 ) ) ;
#876 = ORIENTED_EDGE ( 'NONE', *, *, #5256, .F. ) ;
#877 = CARTESIAN_POINT ( 'NONE',  ( -2.500000000000002220, 0.000000000000000000, 0.000000000000000000 ) ) ;
#878 = CARTESIAN_POINT ( 'NONE',  ( 13.00000000000000178, -3.869963285057273605, 2.986818217332043446 ) ) ;
#879 = EDGE_CURVE ( 'NONE', #7960, #312, #16126, .T. ) ;
#880 = VECTOR ( 'NONE', #12534, 1000.000000000000000 ) ;
#881 = VERTEX_POINT ( 'NONE', #3710 ) ;
#882 = FACE_OUTER_BOUND ( 'NONE', #16027, .T. ) ;
#883 = EDGE_CURVE ( 'NONE', #1239, #4468, #19601, .T. ) ;
#884 = APPLICATION_CONTEXT ( 'automotive_design' ) ;
#885 = DIRECTION ( 'NONE',  ( 1.000000000000000000, 1.224646799147353207E-16, 0.000000000000000000 ) ) ;
#886 = DIRECTION ( 'NONE',  ( -0.000000000000000000, -0.000000000000000000, -1.000000000000000000 ) ) ;
#887 = CARTESIAN_POINT ( 'NONE',  ( 11.34374999795161543, 3.114526743279256049, 3.846120219227944670 ) ) ;
#888 = CARTESIAN_POINT ( 'NONE',  ( 3.476417968967386418, 17.43449690031536292, 32.00000000000000000 ) ) ;
#889 = SURFACE_STYLE_FILL_AREA ( #8496 ) ;
#890 = CARTESIAN_POINT ( 'NONE',  ( 2.765633920072235075, -12.59161484032896361, -21.30679549418645280 ) ) ;
#891 = ORIENTED_EDGE ( 'NONE', *, *, #3139, .T. ) ;
#892 = EDGE_CURVE ( 'NONE', #18407, #15571, #10660, .T. ) ;
#893 = DIRECTION ( 'NONE',  ( 0.000000000000000000, 0.000000000000000000, 1.000000000000000000 ) ) ;
#894 = AXIS2_PLACEMENT_3D ( 'NONE', #13584, #13287, #16392 ) ;
#895 = CARTESIAN_POINT ( 'NONE',  ( 1.899999999999999023, 0.000000000000000000, 0.000000000000000000 ) ) ;
#896 = CARTESIAN_POINT ( 'NONE',  ( 3.814044456245474279, -4.235925505221167064, -13.31249999590322730 ) ) ;
#897 = AXIS2_PLACEMENT_3D ( 'NONE', #9316, #9724, #10914 ) ;
#898 = CARTESIAN_POINT ( 'NONE',  ( 4.233219804643871598, -2.444050593750019651, -11.46874999795161543 ) ) ;
#899 = FACE_OUTER_BOUND ( 'NONE', #11788, .T. ) ;
#900 = ADVANCED_FACE ( 'NONE', ( #16311 ), #10983, .T. ) ;
#901 = ORIENTED_EDGE ( 'NONE', *, *, #9677, .T. ) ;
#902 = CARTESIAN_POINT ( 'NONE',  ( 9.343749997951615427, -3.499494075959840966, 3.499494075959791672 ) ) ;
#903 = CARTESIAN_POINT ( 'NONE',  ( -9.000000000000001776, 1.102182119232617911E-15, -22.00000000000000000 ) ) ;
#904 = ORIENTED_EDGE ( 'NONE', *, *, #7739, .T. ) ;
#905 = CARTESIAN_POINT ( 'NONE',  ( 2.783025306068356741, 18.43727551351032190, 16.17543236987995314 ) ) ;
#906 = DIRECTION ( 'NONE',  ( 1.000000000000000000, 0.000000000000000000, 0.000000000000000000 ) ) ;
#907 = AXIS2_PLACEMENT_3D ( 'NONE', #1856, #14055, #13963 ) ;
#908 = CIRCLE ( 'NONE', #3462, 6.760799999999997034 ) ;
#909 = CARTESIAN_POINT ( 'NONE',  ( -2.647025296874989664, 4.584782303107598267, -6.234374998975811266 ) ) ;
#910 = DIRECTION ( 'NONE',  ( 0.000000000000000000, 0.000000000000000000, 1.000000000000000000 ) ) ;
#911 = EDGE_LOOP ( 'NONE', ( #2200, #15729 ) ) ;
#912 = DIRECTION ( 'NONE',  ( 1.000000000000000000, 0.000000000000000000, 0.000000000000000000 ) ) ;
#913 = DIRECTION ( 'NONE',  ( -1.000000000000000000, 1.224646799147353207E-16, 0.000000000000000000 ) ) ;
#914 = EDGE_CURVE ( 'NONE', #11016, #5140, #8465, .T. ) ;
#915 = DIRECTION ( 'NONE',  ( -0.000000000000000000, -0.000000000000000000, 1.000000000000000000 ) ) ;
#916 = ORIENTED_EDGE ( 'NONE', *, *, #8748, .F. ) ;
#917 =( BOUNDED_CURVE ( )  B_SPLINE_CURVE ( 2, ( #9368, #13668, #1364, #16672, #9267, #19759, #1464, #6048, #12170, #18270, #4558, #56, #6149, #16875, #15372 ),
 .UNSPECIFIED., .F., .F. ) 
 B_SPLINE_CURVE_WITH_KNOTS ( ( 3, 2, 2, 2, 2, 2, 2, 3 ),
 ( 0.000000000000000000, 0.05000000000000000278, 0.1000000000000000056, 0.1499999999999999944, 0.2000000000000000111, 0.2500000000000000000, 0.2999999999999999889, 0.3078686208676164604 ),
 .UNSPECIFIED. ) 
 CURVE ( )  GEOMETRIC_REPRESENTATION_ITEM ( )  RATIONAL_B_SPLINE_CURVE ( ( 1.000000000000000000, 0.9876883405951377704, 1.000000000000000000, 0.9876883405951377704, 1.000000000000000000, 0.9876883405951377704, 1.000000000000000000, 0.9876883405951377704, 1.000000000000000000, 0.9876883405951377704, 1.000000000000000000, 0.9876883405951377704, 1.000000000000000000, 0.9980624843978382899, 0.9967347918236166837 ) ) 
 REPRESENTATION_ITEM ( '' )  );
#918 = CARTESIAN_POINT ( 'NONE',  ( 9.312499995903225525, -5.668774803599153422, -0.5958122406256771697 ) ) ;
#919 = ORIENTED_EDGE ( 'NONE', *, *, #12816, .T. ) ;
#920 = FACE_OUTER_BOUND ( 'NONE', #18601, .T. ) ;
#921 = CARTESIAN_POINT ( 'NONE',  ( 0.02436607992776455150, 5.391175441198956086, -24.15498966839956907 ) ) ;
#922 = PRODUCT_DEFINITION_SHAPE ( 'NONE', 'NONE',  #19799 ) ;
#923 = DIRECTION ( 'NONE',  ( -1.000000000000000000, -0.000000000000000000, -0.000000000000000000 ) ) ;
#924 = VECTOR ( 'NONE', #15469, 1000.000000000000000 ) ;
#925 = DIRECTION ( 'NONE',  ( 1.000000000000000000, -0.000000000000000000, -0.000000000000000000 ) ) ;
#926 = ORIENTED_EDGE ( 'NONE', *, *, #17404, .F. ) ;
#927 = CARTESIAN_POINT ( 'NONE',  ( -11.00000000000000355, 3.278623949159159778, 2.625000000000000888 ) ) ;
#928 = DIRECTION ( 'NONE',  ( -1.000000000000000000, 0.000000000000000000, 0.000000000000000000 ) ) ;
#929 = ORIENTED_EDGE ( 'NONE', *, *, #16286, .T. ) ;
#930 = AXIS2_PLACEMENT_3D ( 'NONE', #8370, #12874, #15974 ) ;
#931 = CARTESIAN_POINT ( 'NONE',  ( 1.734723475976807094E-15, 9.165435523385314198, -0.7089489049740167470 ) ) ;
#932 = DIRECTION ( 'NONE',  ( 1.000000000000000000, 0.000000000000000000, 0.000000000000000000 ) ) ;
#933 = AXIS2_PLACEMENT_3D ( 'NONE', #6535, #2148, #5051 ) ;
#934 = EDGE_LOOP ( 'NONE', ( #9051, #4555 ) ) ;
#935 = DIRECTION ( 'NONE',  ( 0.000000000000000000, 0.000000000000000000, 1.000000000000000000 ) ) ;
#936 = DIRECTION ( 'NONE',  ( 1.000000000000000000, 0.000000000000000000, 0.000000000000000000 ) ) ;
#937 = CARTESIAN_POINT ( 'NONE',  ( 0.000000000000000000, 0.000000000000000000, 35.00000000000000000 ) ) ;
#938 = ADVANCED_FACE ( 'NONE', ( #5984 ), #16710, .F. ) ;
#939 = ORIENTED_EDGE ( 'NONE', *, *, #8365, .F. ) ;
#940 = PLANE ( 'NONE',  #17390 ) ;
#941 = VERTEX_POINT ( 'NONE', #7583 ) ;
#942 = CONTEXT_DEPENDENT_SHAPE_REPRESENTATION ( #9629, #5867 ) ;
#943 = DIRECTION ( 'NONE',  ( 0.000000000000000000, 0.000000000000000000, -1.000000000000000000 ) ) ;
#944 = SURFACE_SIDE_STYLE ('',( #18751 ) ) ;
#945 = LINE ( 'NONE', #13146, #9312 ) ;
#946 = ORIENTED_EDGE ( 'NONE', *, *, #18987, .F. ) ;
#947 = CARTESIAN_POINT ( 'NONE',  ( -2.873153789725852558, -3.954556930911842016, -13.46874999795161543 ) ) ;
#948 = LINE ( 'NONE', #5142, #3038 ) ;
#949 = DIRECTION ( 'NONE',  ( -0.000000000000000000, -0.000000000000000000, 1.000000000000000000 ) ) ;
#950 = ADVANCED_FACE ( 'NONE', ( #16412 ), #6083, .T. ) ;
#951 = ORIENTED_EDGE ( 'NONE', *, *, #13359, .T. ) ;
#952 = CARTESIAN_POINT ( 'NONE',  ( -36.00000000000000000, 1.999999999999998224, -5.000000000000000000 ) ) ;
#953 = ORIENTED_EDGE ( 'NONE', *, *, #8960, .T. ) ;
#954 = EDGE_CURVE ( 'NONE', #8718, #1239, #7054, .T. ) ;
#955 = DIRECTION ( 'NONE',  ( 0.000000000000000000, 0.000000000000000000, 1.000000000000000000 ) ) ;
#956 = CARTESIAN_POINT ( 'NONE',  ( 0.000000000000000000, 0.000000000000000000, 0.000000000000000000 ) ) ;
#957 = EDGE_LOOP ( 'NONE', ( #10118, #13966, #3448, #4840 ) ) ;
#958 = CARTESIAN_POINT ( 'NONE',  ( -3.114526743279308896, -3.846120219227901149, -7.343749997951615427 ) ) ;
#959 = FACE_OUTER_BOUND ( 'NONE', #270, .T. ) ;
#960 = EDGE_LOOP ( 'NONE', ( #14125, #1610 ) ) ;
#961 = ORIENTED_EDGE ( 'NONE', *, *, #11015, .T. ) ;
#962 = CARTESIAN_POINT ( 'NONE',  ( 18.68117051311639543, -3.372863662543048591, 32.00000000000000000 ) ) ;
#963 = CIRCLE ( 'NONE', #1919, 1.000000000000000888 ) ;
#964 = CARTESIAN_POINT ( 'NONE',  ( 12.50000000000000533, -4.840010801796506890, 3.143139765844590983 ) ) ;
#965 = CIRCLE ( 'NONE', #11818, 3.796999999999998820 ) ;
#966 = ADVANCED_FACE ( 'NONE', ( #2687 ), #16816, .F. ) ;
#967 = DIRECTION ( 'NONE',  ( -1.000000000000000000, 0.000000000000000000, 0.000000000000000000 ) ) ;
#968 = ORIENTED_EDGE ( 'NONE', *, *, #18592, .F. ) ;
#969 = DIRECTION ( 'NONE',  ( -1.000000000000000000, -0.000000000000000000, -0.000000000000000000 ) ) ;
#970 = LINE ( 'NONE', #17684, #14905 ) ;
#971 = ORIENTED_EDGE ( 'NONE', *, *, #4682, .F. ) ;
#972 = CARTESIAN_POINT ( 'NONE',  ( 0.006931054464085153848, 2.248820353273311756, -24.42321038836780644 ) ) ;
#973 = CIRCLE ( 'NONE', #3, 3.000000000000000000 ) ;
#974 = AXIS2_PLACEMENT_3D ( 'NONE', #1599, #16821, #7888 ) ;
#975 = CARTESIAN_POINT ( 'NONE',  ( 2.262072769566604080, -11.57956866523201178, -24.43806413951687873 ) ) ;
#976 = CARTESIAN_POINT ( 'NONE',  ( 13.00000000000000178, 0.000000000000000000, 0.000000000000000000 ) ) ;
#977 = EDGE_CURVE ( 'NONE', #5363, #18719, #18306, .T. ) ;
#978 = DIRECTION ( 'NONE',  ( 0.000000000000000000, 0.000000000000000000, 1.000000000000000000 ) ) ;
#979 = EDGE_CURVE ( 'NONE', #11644, #4794, #11939, .T. ) ;
#980 = FACE_OUTER_BOUND ( 'NONE', #5717, .T. ) ;
#981 = SURFACE_STYLE_FILL_AREA ( #8681 ) ;
#982 = DIRECTION ( 'NONE',  ( 0.000000000000000000, 0.000000000000000000, 1.000000000000000000 ) ) ;
#983 = ORIENTED_EDGE ( 'NONE', *, *, #2761, .F. ) ;
#984 = DIRECTION ( 'NONE',  ( 1.000000000000000000, 0.000000000000000000, 0.000000000000000000 ) ) ;
#985 = EDGE_CURVE ( 'NONE', #15288, #59, #8806, .T. ) ;
#986 = DIRECTION ( 'NONE',  ( 0.000000000000000000, 1.000000000000000000, -1.224646799147353207E-16 ) ) ;
#987 = UNCERTAINTY_MEASURE_WITH_UNIT (LENGTH_MEASURE( 1.000000000000000082E-05 ), #1597, 'distance_accuracy_value', 'NONE');
#988 = CARTESIAN_POINT ( 'NONE',  ( 4.465502636338039011, 1.988169868018562436, -8.843749997951615427 ) ) ;
#989 = EDGE_CURVE ( 'NONE', #7371, #2096, #6493, .T. ) ;
#990 = CARTESIAN_POINT ( 'NONE',  ( 3.846120219227923798, -3.114526743279282250, -11.96874999795161365 ) ) ;
#991 = CIRCLE ( 'NONE', #15371, 24.12539914357697768 ) ;
#992 = CARTESIAN_POINT ( 'NONE',  ( -3.270778111535363131, -3.632567103900500971, -10.84374999795161543 ) ) ;
#993 = VERTEX_POINT ( 'NONE', #17908 ) ;
#994 = CARTESIAN_POINT ( 'NONE',  ( 2.789999999999999147, -18.28042085475266276, -15.74360496233401996 ) ) ;
#995 = CARTESIAN_POINT ( 'NONE',  ( 4.235925505221166176, 3.814044456245473835, -8.312499995903225525 ) ) ;
#996 = ORIENTED_EDGE ( 'NONE', *, *, #13001, .F. ) ;
#997 = CARTESIAN_POINT ( 'NONE',  ( 2.765633920072235519, 18.55949924794892780, 16.37294372382865504 ) ) ;
#998 = DIRECTION ( 'NONE',  ( -1.000000000000000000, 0.000000000000000000, 0.000000000000000000 ) ) ;
#999 = CARTESIAN_POINT ( 'NONE',  ( 2.789999999999999147, -15.74360496233394002, 18.28042085475272671 ) ) ;
#1000 = ORIENTED_EDGE ( 'NONE', *, *, #10017, .T. ) ;
#1001 = AXIS2_PLACEMENT_3D ( 'NONE', #3476, #9794, #9585 ) ;
#1002 = DIRECTION ( 'NONE',  ( 0.000000000000000000, 0.4999999999999920619, 0.8660254037844432595 ) ) ;
#1003 = CARTESIAN_POINT ( 'NONE',  ( 2.601776121706764311, -19.18368891937477727, -17.47009390565512632 ) ) ;
#1004 = DIRECTION ( 'NONE',  ( 0.000000000000000000, 0.000000000000000000, -1.000000000000000000 ) ) ;
#1005 = ORIENTED_EDGE ( 'NONE', *, *, #11824, .F. ) ;
#1006 = ORIENTED_EDGE ( 'NONE', *, *, #16529, .F. ) ;
#1007 = CARTESIAN_POINT ( 'NONE',  ( 1.039999999999997371, -4.147968289691092991, -27.76164181293055933 ) ) ;
#1008 = EDGE_CURVE ( 'NONE', #9627, #14187, #12006, .T. ) ;
#1009 = CARTESIAN_POINT ( 'NONE',  ( 1.255998204157470211, -17.85806462366060288, 32.00000000000000000 ) ) ;
#1010 = EDGE_CURVE ( 'NONE', #11279, #809, #19496, .T. ) ;
#1011 = DIRECTION ( 'NONE',  ( -1.000000000000000000, 0.000000000000000000, 0.000000000000000000 ) ) ;
#1012 = CARTESIAN_POINT ( 'NONE',  ( -3.350375938067097437, 4.611396867937201272, -9.000000000000005329 ) ) ;
#1013 = VERTEX_POINT ( 'NONE', #5784 ) ;
#1014 = FACE_BOUND ( 'NONE', #7800, .T. ) ;
#1015 = CARTESIAN_POINT ( 'NONE',  ( 2.789999999999999147, -2.336989772644440855, 24.63872515616082026 ) ) ;
#1016 = AXIS2_PLACEMENT_3D ( 'NONE', #3831, #10049, #2613 ) ;
#1017 = ORIENTED_EDGE ( 'NONE', *, *, #19676, .T. ) ;
#1018 = TOROIDAL_SURFACE ( 'NONE', #19533, 6.760799999999997034, 0.03079999999999868954 ) ;
#1019 = EDGE_CURVE ( 'NONE', #15780, #17520, #11302, .T. ) ;
#1020 = AXIS2_PLACEMENT_3D ( 'NONE', #13409, #7495, #5603 ) ;
#1021 = CARTESIAN_POINT ( 'NONE',  ( 2.624839991567102793, 7.649983447674348902, -0.06756670027993921801 ) ) ;
#1022 = CARTESIAN_POINT ( 'NONE',  ( -0.5958122406255597081, 5.668774803599165857, -14.00000000000000533 ) ) ;
#1023 = EDGE_CURVE ( 'NONE', #1471, #15059, #3313, .T. ) ;
#1024 = ORIENTED_EDGE ( 'NONE', *, *, #3666, .F. ) ;
#1025 = CARTESIAN_POINT ( 'NONE',  ( 2.850000000000024070, 4.936344801571289409, -6.000000000000005329 ) ) ;
#1026 = CARTESIAN_POINT ( 'NONE',  ( 5.699999596629369059, -0.002144393866035136480, -6.000593838912648081 ) ) ;
#1027 = ADVANCED_FACE ( 'NONE', ( #17294 ), #1697, .F. ) ;
#1028 = FACE_OUTER_BOUND ( 'NONE', #19195, .T. ) ;
#1029 = B_SPLINE_CURVE_WITH_KNOTS ( 'NONE', 3,
 ( #17819, #16318, #7089, #16224 ),
 .UNSPECIFIED., .F., .F.,
 ( 4, 4 ),
 ( 1.981826382900813409E-07, 0.0006887856082032216450 ),
 .UNSPECIFIED. ) ;
#1030 = ORIENTED_EDGE ( 'NONE', *, *, #6750, .F. ) ;
#1031 = FACE_OUTER_BOUND ( 'NONE', #12382, .T. ) ;
#1032 = ORIENTED_EDGE ( 'NONE', *, *, #7222, .T. ) ;
#1033 = DIRECTION ( 'NONE',  ( -1.000000000000000000, 0.000000000000000000, -0.000000000000000000 ) ) ;
#1034 = AXIS2_PLACEMENT_3D ( 'NONE', #3290, #9404, #10094 ) ;
#1035 = ORIENTED_EDGE ( 'NONE', *, *, #8366, .F. ) ;
#1036 = VECTOR ( 'NONE', #16677, 1000.000000000000000 ) ;
#1037 = CARTESIAN_POINT ( 'NONE',  ( 11.96874999795161365, -3.114526743279282250, 3.846120219227923798 ) ) ;
#1038 = CARTESIAN_POINT ( 'NONE',  ( 2.257825491203655943, -24.44564404695836402, -11.58891744060133355 ) ) ;
#1039 = TOROIDAL_SURFACE ( 'NONE', #8382, 24.12539914357697768, 8.000000000000000000 ) ;
#1040 = CARTESIAN_POINT ( 'NONE',  ( -10.99900000000000233, 4.200000000000000178, 5.143516556418882928E-16 ) ) ;
#1041 = VERTEX_POINT ( 'NONE', #3291 ) ;
#1042 = DIRECTION ( 'NONE',  ( -0.000000000000000000, -0.000000000000000000, 1.000000000000000000 ) ) ;
#1043 = FACE_OUTER_BOUND ( 'NONE', #16772, .T. ) ;
#1044 = FACE_OUTER_BOUND ( 'NONE', #18531, .T. ) ;
#1045 = EDGE_LOOP ( 'NONE', ( #18049, #2720, #5129, #19018 ) ) ;
#1046 = AXIS2_PLACEMENT_3D ( 'NONE', #7959, #6258, #16985 ) ;
#1047 = DIRECTION ( 'NONE',  ( -1.000000000000000000, 0.000000000000000000, 0.000000000000000000 ) ) ;
#1048 = EDGE_CURVE ( 'NONE', #10126, #13404, #8108, .T. ) ;
#1049 = TOROIDAL_SURFACE ( 'NONE', #4235, 24.12539914357697768, 8.000000000000000000 ) ;
#1050 = ORIENTED_EDGE ( 'NONE', *, *, #3700, .F. ) ;
#1051 = AXIS2_PLACEMENT_3D ( 'NONE', #541, #6513, #1831 ) ;
#1052 = EDGE_CURVE ( 'NONE', #11676, #59, #3252, .T. ) ;
#1053 = CIRCLE ( 'NONE', #13502, 1.199999999999999734 ) ;
#1054 = CARTESIAN_POINT ( 'NONE',  ( 0.006931069955679000985, 16.17493693894905959, -18.43696893154741190 ) ) ;
#1055 = EDGE_CURVE ( 'NONE', #11999, #7717, #12788, .T. ) ;
#1056 = AXIS2_PLACEMENT_3D ( 'NONE', #2528, #10810, #9310 ) ;
#1057 = CARTESIAN_POINT ( 'NONE',  ( 2.765633920072238627, -21.30679549418621832, -12.59161484032935618 ) ) ;
#1058 = EDGE_LOOP ( 'NONE', ( #17820, #7756, #19150, #14489 ) ) ;
#1059 = CARTESIAN_POINT ( 'NONE',  ( -4.233219804643852946, 2.444050593750049405, -11.84374999795161365 ) ) ;
#1060 = FILL_AREA_STYLE ('',( #17574 ) ) ;
#1061 = CARTESIAN_POINT ( 'NONE',  ( 2.695436003842732298, 4.150607464521791634, -9.968749997951617203 ) ) ;
#1062 = ORIENTED_EDGE ( 'NONE', *, *, #10676, .F. ) ;
#1063 = ORIENTED_EDGE ( 'NONE', *, *, #9677, .F. ) ;
#1064 = DIRECTION ( 'NONE',  ( 0.000000000000000000, 0.000000000000000000, 1.000000000000000000 ) ) ;
#1065 = MECHANICAL_DESIGN_GEOMETRIC_PRESENTATION_REPRESENTATION (  '', ( #9705 ), #3287 ) ;
#1066 = EDGE_CURVE ( 'NONE', #1381, #19705, #15773, .T. ) ;
#1067 = CARTESIAN_POINT ( 'NONE',  ( 11.00000000000000711, -2.850000000000023626, 4.936344801571289409 ) ) ;
#1068 = ORIENTED_EDGE ( 'NONE', *, *, #3459, .T. ) ;
#1069 = CARTESIAN_POINT ( 'NONE',  ( 0.1855657389739088781, -25.39738473785004302, 5.253342437939627629 ) ) ;
#1070 = ORIENTED_EDGE ( 'NONE', *, *, #3622, .F. ) ;
#1071 = DIRECTION ( 'NONE',  ( 0.000000000000000000, 0.000000000000000000, -1.000000000000000000 ) ) ;
#1072 = AXIS2_PLACEMENT_3D ( 'NONE', #18591, #15796, #15599 ) ;
#1073 = B_SPLINE_CURVE_WITH_KNOTS ( 'NONE', 1,
 ( #8978, #2969 ),
 .UNSPECIFIED., .F., .F.,
 ( 2, 2 ),
 ( 0.000000000000000000, 1.000000000000000000 ),
 .UNSPECIFIED. ) ;
#1074 = CARTESIAN_POINT ( 'NONE',  ( 15.19790265903627358, 9.644882309621939598, 32.00000000000000000 ) ) ;
#1075 = ORIENTED_EDGE ( 'NONE', *, *, #15150, .T. ) ;
#1076 = CARTESIAN_POINT ( 'NONE',  ( -14.86923836996421144, -11.47363181547641275, 35.00000000000000000 ) ) ;
#1077 = PRESENTATION_LAYER_ASSIGNMENT (  '', '', ( #9723 ) ) ;
#1078 = ADVANCED_FACE ( 'NONE', ( #7789 ), #290, .T. ) ;
#1079 = CARTESIAN_POINT ( 'NONE',  ( -13.86923836996420967, -11.47363181547641275, 32.00000000000000000 ) ) ;
#1080 = CARTESIAN_POINT ( 'NONE',  ( 12.84374999795161543, 4.648860486681953397, 1.510506337161861223 ) ) ;
#1081 = CARTESIAN_POINT ( 'NONE',  ( 9.343749997951615427, 4.780397808154257078, 1.280903732194454081 ) ) ;
#1082 = PRODUCT_DEFINITION_SHAPE ( 'NONE', 'NONE',  #11510 ) ;
#1083 = DIRECTION ( 'NONE',  ( -1.000000000000000000, -1.224646799147353207E-16, 0.000000000000000000 ) ) ;
#1084 = CARTESIAN_POINT ( 'NONE',  ( 17.68117051311639898, -3.372863662543048591, 35.00000000000000000 ) ) ;
#1085 = TOROIDAL_SURFACE ( 'NONE', #19621, 8.239200000000002078, 0.03079999999999868954 ) ;
#1086 = EDGE_LOOP ( 'NONE', ( #14105, #10699, #4262, #2894, #2428, #15632, #5816, #10568 ) ) ;
#1087 = CARTESIAN_POINT ( 'NONE',  ( 0.000000000000000000, 0.000000000000000000, -35.00000000000000000 ) ) ;
#1088 = DIRECTION ( 'NONE',  ( -1.000000000000000000, 0.000000000000000000, 0.000000000000000000 ) ) ;
#1089 = FACE_OUTER_BOUND ( 'NONE', #11558, .T. ) ;
#1090 = DIRECTION ( 'NONE',  ( 0.000000000000000000, 0.000000000000000000, 1.000000000000000000 ) ) ;
#1091 = STYLED_ITEM ( 'NONE', ( #13477 ), #4233 ) ;
#1092 = VECTOR ( 'NONE', #14739, 1000.000000000000000 ) ;
#1093 = CARTESIAN_POINT ( 'NONE',  ( -4.080749450109650844, 4.080749450109650844, -9.812499995903223748 ) ) ;
#1094 = ADVANCED_FACE ( 'NONE', ( #3490 ), #10996, .F. ) ;
#1095 = ORIENTED_EDGE ( 'NONE', *, *, #14831, .F. ) ;
#1096 = CARTESIAN_POINT ( 'NONE',  ( 0.07186808533286581646, -23.19485392143207036, -10.24630254990540834 ) ) ;
#1097 = ADVANCED_FACE ( 'NONE', ( #9600 ), #1889, .F. ) ;
#1098 = DIRECTION ( 'NONE',  ( 1.000000000000000000, 0.000000000000000000, 0.000000000000000000 ) ) ;
#1099 = EDGE_LOOP ( 'NONE', ( #1954, #16438, #575, #16915 ) ) ;
#1100 = CARTESIAN_POINT ( 'NONE',  ( 9.468749997951615427, -0.5109457054261099529, -4.861323657744413218 ) ) ;
#1101 = CIRCLE ( 'NONE', #14213, 12.00000000000000178 ) ;
#1102 = CARTESIAN_POINT ( 'NONE',  ( 2.789999999999999147, -24.44424927289185590, -0.2301004812060095106 ) ) ;
#1103 = EDGE_CURVE ( 'NONE', #13293, #13685, #7982, .T. ) ;
#1104 = EDGE_CURVE ( 'NONE', #17455, #298, #6560, .T. ) ;
#1105 = CARTESIAN_POINT ( 'NONE',  ( 0.000000000000000000, 5.535312321043032391, -23.48180575137725867 ) ) ;
#1106 = CARTESIAN_POINT ( 'NONE',  ( -5.700000000000002842, 0.000000000000000000, -18.00000000000000355 ) ) ;
#1107 = VERTEX_POINT ( 'NONE', #4987 ) ;
#1108 = AXIS2_PLACEMENT_3D ( 'NONE', #4038, #19235, #5530 ) ;
#1109 = CARTESIAN_POINT ( 'NONE',  ( -19.00000000000000355, -4.200000000000000178, 0.000000000000000000 ) ) ;
#1110 = CARTESIAN_POINT ( 'NONE',  ( 10.00000000000000533, -5.421022142882388373, 1.761396867937162769 ) ) ;
#1111 = ORIENTED_EDGE ( 'NONE', *, *, #11893, .T. ) ;
#1112 = CARTESIAN_POINT ( 'NONE',  ( 0.000000000000000000, 0.000000000000000000, -29.00000000000000000 ) ) ;
#1113 = ORIENTED_EDGE ( 'NONE', *, *, #17514, .F. ) ;
#1114 = CARTESIAN_POINT ( 'NONE',  ( 9.468749997951615427, -3.954556930911881985, 2.873153789725797491 ) ) ;
#1115 = CIRCLE ( 'NONE', #11348, 1.000000000000004441 ) ;
#1116 = CARTESIAN_POINT ( 'NONE',  ( 17.96448111170888851, 1.130229351527639148, 35.00000000000000000 ) ) ;
#1117 = DIRECTION ( 'NONE',  ( -1.000000000000000000, 0.000000000000000000, 0.000000000000000000 ) ) ;
#1118 = ADVANCED_BREP_SHAPE_REPRESENTATION ( '', ( #16042, #16724 ), #279 ) ;
#1119 = CARTESIAN_POINT ( 'NONE',  ( 4.611396867937200383, 3.350375938067097881, -14.00000000000000533 ) ) ;
#1120 = VERTEX_POINT ( 'NONE', #1984 ) ;
#1121 = DIRECTION ( 'NONE',  ( 0.000000000000000000, 0.000000000000000000, -1.000000000000000000 ) ) ;
#1122 = DIRECTION ( 'NONE',  ( 0.000000000000000000, 1.224646799147367998E-16, 1.000000000000000000 ) ) ;
#1123 = AXIS2_PLACEMENT_3D ( 'NONE', #10070, #11847, #2733 ) ;
#1124 = ORIENTED_EDGE ( 'NONE', *, *, #12744, .T. ) ;
#1125 = EDGE_CURVE ( 'NONE', #3988, #14268, #7776, .T. ) ;
#1126 = DIRECTION ( 'NONE',  ( 1.000000000000000000, -0.000000000000000000, -0.000000000000000000 ) ) ;
#1127 = CARTESIAN_POINT ( 'NONE',  ( 0.07181524296601557444, 18.89296398180216130, -16.91181672897712929 ) ) ;
#1128 = EDGE_CURVE ( 'NONE', #12550, #10762, #14243, .T. ) ;
#1129 = VERTEX_POINT ( 'NONE', #6182 ) ;
#1130 = CARTESIAN_POINT ( 'NONE',  ( 4.840010801796506001, 3.143139765844590983, -7.500000000000005329 ) ) ;
#1131 = FACE_OUTER_BOUND ( 'NONE', #13815, .T. ) ;
#1132 = FACE_OUTER_BOUND ( 'NONE', #17975, .T. ) ;
#1133 = ORIENTED_EDGE ( 'NONE', *, *, #15532, .F. ) ;
#1134 = DIRECTION ( 'NONE',  ( 0.000000000000000000, 0.000000000000000000, 1.000000000000000000 ) ) ;
#1135 = EDGE_LOOP ( 'NONE', ( #157, #14913, #6310, #14769 ) ) ;
#1136 = CARTESIAN_POINT ( 'NONE',  ( 13.00000000000000000, 1.727010089215937905, 5.432074755721460591 ) ) ;
#1137 = VECTOR ( 'NONE', #2464, 1000.000000000000000 ) ;
#1138 = ORIENTED_EDGE ( 'NONE', *, *, #8534, .T. ) ;
#1139 = CARTESIAN_POINT ( 'NONE',  ( 7.968749997951616315, 2.695436003842704764, 4.150607464521812062 ) ) ;
#1140 = CARTESIAN_POINT ( 'NONE',  ( 1.749999999999998002, -27.68468304288262516, 4.633866840648810381 ) ) ;
#1141 = CIRCLE ( 'NONE', #6870, 24.12539914357697413 ) ;
#1142 = DIRECTION ( 'NONE',  ( 1.000000000000000000, 0.000000000000000000, 0.000000000000000000 ) ) ;
#1143 = EDGE_CURVE ( 'NONE', #7513, #15780, #9300, .T. ) ;
#1144 = CARTESIAN_POINT ( 'NONE',  ( -3.954556930911881096, -2.873153789725797935, -14.46874999795161720 ) ) ;
#1145 = CARTESIAN_POINT ( 'NONE',  ( 8.500000000000007105, -5.574407415329147852, -1.493657965219562511 ) ) ;
#1146 = CARTESIAN_POINT ( 'NONE',  ( -4.465502636338010589, 1.988169868018623720, -14.84374999795161543 ) ) ;
#1147 = EDGE_LOOP ( 'NONE', ( #4096, #3789, #12811, #6049 ) ) ;
#1148 = EDGE_CURVE ( 'NONE', #5529, #11664, #6279, .T. ) ;
#1150 = ADVANCED_FACE ( 'NONE', ( #6371 ), #5472, .F. ) ;
#1149 = EDGE_CURVE ( 'NONE', #19757, #19457, #12600, .T. ) ;
#1151 = DIRECTION ( 'NONE',  ( 1.000000000000000000, 0.000000000000000000, 0.000000000000000000 ) ) ;
#1152 = AXIS2_PLACEMENT_3D ( 'NONE', #13149, #10064, #16167 ) ;
#1153 = ORIENTED_EDGE ( 'NONE', *, *, #6590, .T. ) ;
#1154 = CARTESIAN_POINT ( 'NONE',  ( 17.11901729331276556, 5.562305898749055011, -35.00000000000000000 ) ) ;
#1155 = FACE_OUTER_BOUND ( 'NONE', #17530, .T. ) ;
#1156 = CARTESIAN_POINT ( 'NONE',  ( 0.000000000000000000, 0.000000000000000000, -6.000000000000005329 ) ) ;
#1157 = ORIENTED_EDGE ( 'NONE', *, *, #5900, .F. ) ;
#1158 = CARTESIAN_POINT ( 'NONE',  ( 4.465502636338025688, -1.988169868018592856, -14.46874999795161720 ) ) ;
#1159 = CARTESIAN_POINT ( 'NONE',  ( -3.469446951953614189E-15, 3.035766082959412415E-15, -37.00000000000000711 ) ) ;
#1160 = CARTESIAN_POINT ( 'NONE',  ( 0.5958122406256377568, 5.668774803599156975, -9.312499995903225525 ) ) ;
#1161 = ORIENTED_EDGE ( 'NONE', *, *, #6150, .T. ) ;
#1162 = VERTEX_POINT ( 'NONE', #3983 ) ;
#1163 = DIRECTION ( 'NONE',  ( 1.000000000000000000, 0.000000000000000000, 0.000000000000000000 ) ) ;
#1164 = CIRCLE ( 'NONE', #6254, 5.200000000000000178 ) ;
#1165 = CARTESIAN_POINT ( 'NONE',  ( 11.50000000000000355, -3.631840208645826351, 4.484949146646356688 ) ) ;
#1166 = CIRCLE ( 'NONE', #11076, 6.500000000000000000 ) ;
#1167 = ORIENTED_EDGE ( 'NONE', *, *, #17905, .T. ) ;
#1168 = CARTESIAN_POINT ( 'NONE',  ( 1.039999999999997149, -27.68468304288261805, 4.633866840648821039 ) ) ;
#1169 = EDGE_LOOP ( 'NONE', ( #12727, #1613 ) ) ;
#1170 = DIRECTION ( 'NONE',  ( -0.000000000000000000, -0.000000000000000000, 1.000000000000000000 ) ) ;
#1171 = DIRECTION ( 'NONE',  ( -1.000000000000000000, -0.000000000000000000, -0.000000000000000000 ) ) ;
#1172 = ORIENTED_EDGE ( 'NONE', *, *, #662, .F. ) ;
#1173 = CARTESIAN_POINT ( 'NONE',  ( 1.774186184918758212E-16, 2.133490293297354956, -24.22479935914658000 ) ) ;
#1174 = AXIS2_PLACEMENT_3D ( 'NONE', #14507, #5380, #8288 ) ;
#1175 = CIRCLE ( 'NONE', #9821, 1.000000000000004441 ) ;
#1176 = DIRECTION ( 'NONE',  ( 0.000000000000000000, 0.000000000000000000, -1.000000000000000000 ) ) ;
#1177 = CARTESIAN_POINT ( 'NONE',  ( 11.31249999590322375, 5.421022142882375938, -1.761396867937200739 ) ) ;
#1178 = DIRECTION ( 'NONE',  ( -1.000000000000000000, -0.000000000000000000, -0.000000000000000000 ) ) ;
#1179 = DIRECTION ( 'NONE',  ( -1.000000000000000000, 0.000000000000000000, -0.000000000000000000 ) ) ;
#1180 =( NAMED_UNIT ( * ) SI_UNIT ( $, .STERADIAN. ) SOLID_ANGLE_UNIT ( ) );
#1181 = FACE_OUTER_BOUND ( 'NONE', #3715, .T. ) ;
#1182 = ORIENTED_EDGE ( 'NONE', *, *, #6055, .F. ) ;
#1183 = FACE_OUTER_BOUND ( 'NONE', #8230, .T. ) ;
#1184 = DIRECTION ( 'NONE',  ( -1.000000000000000000, -0.000000000000000000, -0.000000000000000000 ) ) ;
#1185 = UNCERTAINTY_MEASURE_WITH_UNIT (LENGTH_MEASURE( 1.000000000000000082E-05 ), #18893, 'distance_accuracy_value', 'NONE');
#1186 = DIRECTION ( 'NONE',  ( -1.000000000000000000, 0.000000000000000000, 0.000000000000000000 ) ) ;
#1187 = CARTESIAN_POINT ( 'NONE',  ( 2.765633920072235519, -9.836394144775869819, 22.71065055754449347 ) ) ;
#1188 = B_SPLINE_CURVE_WITH_KNOTS ( 'NONE', 3,
 ( #16068, #17851, #14568, #4147, #2833, #10651 ),
 .UNSPECIFIED., .F., .F.,
 ( 4, 2, 4 ),
 ( 1.979325885386966398E-07, 0.001878588715165604951, 0.003756979497742671432 ),
 .UNSPECIFIED. ) ;
#1189 = CIRCLE ( 'NONE', #19389, 7.937500000000000000 ) ;
#1190 = CARTESIAN_POINT ( 'NONE',  ( 12.99999999999999467, 4.496324317583058949, 1.917446440021246756 ) ) ;
#1191 = ADVANCED_FACE ( 'NONE', ( #6964 ), #14504, .T. ) ;
#1192 = AXIS2_PLACEMENT_3D ( 'NONE', #12017, #18122, #12117 ) ;
#1193 = ORIENTED_EDGE ( 'NONE', *, *, #3422, .T. ) ;
#1194 = DIRECTION ( 'NONE',  ( 1.000000000000000000, 0.000000000000000000, 0.000000000000000000 ) ) ;
#1195 = CARTESIAN_POINT ( 'NONE',  ( 0.5958122406255995651, -5.668774803599162304, -14.00000000000000533 ) ) ;
#1196 = EDGE_LOOP ( 'NONE', ( #11214, #10475, #18129, #3079 ) ) ;
#1197 = FACE_OUTER_BOUND ( 'NONE', #635, .T. ) ;
#1198 = LINE ( 'NONE', #9203, #10258 ) ;
#1199 = CARTESIAN_POINT ( 'NONE',  ( 0.1855656748306449277, 2.851997810082009366, -25.77772010606602748 ) ) ;
#1200 = CARTESIAN_POINT ( 'NONE',  ( 2.789999999999999147, -19.64056340710884996, 14.55412442567610931 ) ) ;
#1201 = EDGE_LOOP ( 'NONE', ( #15506, #1113, #10005, #6475 ) ) ;
#1202 = DIRECTION ( 'NONE',  ( 1.000000000000000000, 0.000000000000000000, 0.000000000000000000 ) ) ;
#1203 = CARTESIAN_POINT ( 'NONE',  ( -9.580134541264520465, -14.56230589874905235, -32.00000000000000000 ) ) ;
#1204 = TOROIDAL_SURFACE ( 'NONE', #572, 24.12539914357697768, 8.000000000000000000 ) ;
#1205 = EDGE_CURVE ( 'NONE', #10763, #9786, #692, .T. ) ;
#1206 = CARTESIAN_POINT ( 'NONE',  ( 4.888101187500000222, -3.413342815706642518E-14, -6.468749997951615427 ) ) ;
#1207 = VERTEX_POINT ( 'NONE', #9905 ) ;
#1208 = CARTESIAN_POINT ( 'NONE',  ( 2.789999999999999147, -15.04425356660744839, -18.18163861606288378 ) ) ;
#1209 = ORIENTED_EDGE ( 'NONE', *, *, #3804, .F. ) ;
#1210 = CARTESIAN_POINT ( 'NONE',  ( -0.6476140635210462237, 8.791535369480451223, -0.4930775504667659903 ) ) ;
#1211 = CARTESIAN_POINT ( 'NONE',  ( 12.84374999795161543, 4.648860486681953397, 1.510506337161861223 ) ) ;
#1212 = CARTESIAN_POINT ( 'NONE',  ( 0.02436607992776194942, -5.391175441198450713, -24.15498966839968276 ) ) ;
#1213 = CYLINDRICAL_SURFACE ( 'NONE', #12720, 0.9999999999999974465 ) ;
#1214 = EDGE_CURVE ( 'NONE', #11454, #10545, #2469, .T. ) ;
#1215 = VERTEX_POINT ( 'NONE', #19085 ) ;
#1216 = DIRECTION ( 'NONE',  ( 1.000000000000000000, 0.000000000000000000, 0.000000000000000000 ) ) ;
#1217 = CARTESIAN_POINT ( 'NONE',  ( 11.31249999590322375, -1.185096637661254171, 5.575441324182689229 ) ) ;
#1218 = CIRCLE ( 'NONE', #9208, 24.12539914357697413 ) ;
#1219 = VERTEX_POINT ( 'NONE', #14599 ) ;
#1220 = CIRCLE ( 'NONE', #15590, 1.000000000000000000 ) ;
#1221 = CYLINDRICAL_SURFACE ( 'NONE', #6122, 13.19999999999999929 ) ;
#1222 = CARTESIAN_POINT ( 'NONE',  ( 1.000000000000003331, 18.00000000000000355, -32.00000000000000000 ) ) ;
#1223 = EDGE_LOOP ( 'NONE', ( #18942, #10771, #450, #12959 ) ) ;
#1224 = CARTESIAN_POINT ( 'NONE',  ( 4.620319390059829168, 1.773574444220725299, -11.96874999795161365 ) ) ;
#1225 = CARTESIAN_POINT ( 'NONE',  ( -5.476417968967388639, 17.43449690031536292, 35.00000000000000000 ) ) ;
#1226 = CARTESIAN_POINT ( 'NONE',  ( 0.001869172971454433714, -20.90869469097853894, -12.51925356660784594 ) ) ;
#1227 = ORIENTED_EDGE ( 'NONE', *, *, #12892, .T. ) ;
#1228 = EDGE_CURVE ( 'NONE', #3208, #2962, #13744, .T. ) ;
#1229 = CARTESIAN_POINT ( 'NONE',  ( -3.207603742328077057E-13, 82.80384757729329692, 37.99999999999999289 ) ) ;
#1230 = VERTEX_POINT ( 'NONE', #16099 ) ;
#1232 = CARTESIAN_POINT ( 'NONE',  ( 1.749999999999998002, 20.02152543075346003, 19.67366047555537634 ) ) ;
#1231 = AXIS2_PLACEMENT_3D ( 'NONE', #15069, #1363, #7441 ) ;
#1233 = ORIENTED_EDGE ( 'NONE', *, *, #17608, .T. ) ;
#1234 = CARTESIAN_POINT ( 'NONE',  ( 2.765633920072235963, -16.37294372382871188, 18.55949924794887096 ) ) ;
#1235 = CARTESIAN_POINT ( 'NONE',  ( -3.499494075959840078, -3.499494075959791672, -14.34374999795161365 ) ) ;
#1236 = CARTESIAN_POINT ( 'NONE',  ( 11.46874999795161543, -2.444050593749961031, -4.233219804643904460 ) ) ;
#1237 = EDGE_CURVE ( 'NONE', #8660, #11518, #6111, .T. ) ;
#1238 = DIRECTION ( 'NONE',  ( 1.000000000000000000, 0.000000000000000000, 0.000000000000000000 ) ) ;
#1239 = VERTEX_POINT ( 'NONE', #14691 ) ;
#1240 = CARTESIAN_POINT ( 'NONE',  ( 1.749999999999998002, 12.96210679857786552, 24.89775460606837143 ) ) ;
#1241 = ADVANCED_FACE ( 'NONE', ( #2565 ), #8492, .T. ) ;
#1242 =( NAMED_UNIT ( * ) PLANE_ANGLE_UNIT ( ) SI_UNIT ( $, .RADIAN. ) );
#1243 = PRODUCT ( 'brake cone', 'brake cone', '', ( #7842 ) ) ;
#1244 = VECTOR ( 'NONE', #3600, 1000.000000000000000 ) ;
#1245 = ORIENTED_EDGE ( 'NONE', *, *, #9812, .F. ) ;
#1246 = LINE ( 'NONE', #7323, #46 ) ;
#1247 = EDGE_CURVE ( 'NONE', #19695, #4381, #18662, .T. ) ;
#1248 = CYLINDRICAL_SURFACE ( 'NONE', #7349, 13.19999999999999929 ) ;
#1249 = CARTESIAN_POINT ( 'NONE',  ( -16.11901729331276911, 5.562305898749051458, -32.00000000000000000 ) ) ;
#1250 = AXIS2_PLACEMENT_3D ( 'NONE', #13559, #19660, #1553 ) ;
#1251 = LINE ( 'NONE', #2941, #13207 ) ;
#1252 = ORIENTED_EDGE ( 'NONE', *, *, #2254, .T. ) ;
#1253 = CARTESIAN_POINT ( 'NONE',  ( 12.73273607671833929, -0.6164700669140440459, -4.866269517993464078 ) ) ;
#1254 = ORIENTED_EDGE ( 'NONE', *, *, #6270, .F. ) ;
#1255 = EDGE_CURVE ( 'NONE', #12054, #5418, #5238, .T. ) ;
#1256 = CARTESIAN_POINT ( 'NONE',  ( -0.3020334839682475847, 5.763142191869157216, -7.500000000000005329 ) ) ;
#1257 = CARTESIAN_POINT ( 'NONE',  ( 2.765633920072235519, -9.836394144775869819, 22.71065055754449347 ) ) ;
#1258 = EDGE_CURVE ( 'NONE', #13729, #18135, #15151, .T. ) ;
#1259 = ORIENTED_EDGE ( 'NONE', *, *, #6877, .F. ) ;
#1260 = EDGE_LOOP ( 'NONE', ( #13516, #17218, #40, #9749 ) ) ;
#1261 = CYLINDRICAL_SURFACE ( 'NONE', #273, 1.000000000000004441 ) ;
#1262 = AXIS2_PLACEMENT_3D ( 'NONE', #8364, #8469, #862 ) ;
#1263 = CARTESIAN_POINT ( 'NONE',  ( 9.000000000000005329, 0.5958122406255991210, 5.668774803599163192 ) ) ;
#1264 = VERTEX_POINT ( 'NONE', #5570 ) ;
#1265 =( GEOMETRIC_REPRESENTATION_CONTEXT ( 3 ) GLOBAL_UNCERTAINTY_ASSIGNED_CONTEXT ( ( #3992 ) ) GLOBAL_UNIT_ASSIGNED_CONTEXT ( ( #19051, #2529, #14656 ) ) REPRESENTATION_CONTEXT ( 'NONE', 'WORKASPACE' ) );
#1266 = DIRECTION ( 'NONE',  ( 0.000000000000000000, 0.000000000000000000, 1.000000000000000000 ) ) ;
#1267 = ORIENTED_EDGE ( 'NONE', *, *, #7190, .F. ) ;
#1268 = DIRECTION ( 'NONE',  ( 1.000000000000000000, 0.000000000000000000, 0.000000000000000000 ) ) ;
#1269 = CARTESIAN_POINT ( 'NONE',  ( 1.999999999999998668, -8.000000000000003553, 37.99999999999999289 ) ) ;
#1270 = EDGE_LOOP ( 'NONE', ( #9959, #8302, #10280, #10813 ) ) ;
#1271 = EDGE_CURVE ( 'NONE', #9660, #13659, #16197, .T. ) ;
#1272 = EDGE_CURVE ( 'NONE', #16734, #11638, #15911, .T. ) ;
#1273 = CARTESIAN_POINT ( 'NONE',  ( 17.96448111170888851, 1.130229351527639148, 32.00000000000000000 ) ) ;
#1274 = DIRECTION ( 'NONE',  ( -1.000000000000000000, 0.000000000000000000, -0.000000000000000000 ) ) ;
#1275 = CARTESIAN_POINT ( 'NONE',  ( -2.000000000000001776, -3.950217066951263956, -3.681818181818183877 ) ) ;
#1276 = ADVANCED_FACE ( 'NONE', ( #9805 ), #15898, .F. ) ;
#1277 = TOROIDAL_SURFACE ( 'NONE', #5732, 6.000000000000000000, 1.199999999999999956 ) ;
#1278 = VERTEX_POINT ( 'NONE', #11394 ) ;
#1279 = DIRECTION ( 'NONE',  ( -1.000000000000000000, -0.000000000000000000, -0.000000000000000000 ) ) ;
#1280 = AXIS2_PLACEMENT_3D ( 'NONE', #15135, #2719, #4426 ) ;
#1281 = DIRECTION ( 'NONE',  ( 0.000000000000000000, 0.000000000000000000, -1.000000000000000000 ) ) ;
#1282 = B_SPLINE_CURVE_WITH_KNOTS ( 'NONE', 3,
 ( #13247, #11275, #6547, #17273 ),
 .UNSPECIFIED., .F., .F.,
 ( 4, 4 ),
 ( 0.005258120783916793266, 0.005948386350302923772 ),
 .UNSPECIFIED. ) ;
#1283 = ORIENTED_EDGE ( 'NONE', *, *, #10304, .T. ) ;
#1284 = DIRECTION ( 'NONE',  ( 0.000000000000000000, 0.000000000000000000, 1.000000000000000000 ) ) ;
#1285 = FACE_BOUND ( 'NONE', #3109, .T. ) ;
#1286 = DIRECTION ( 'NONE',  ( -0.000000000000000000, -0.000000000000000000, 1.000000000000000000 ) ) ;
#1287 = CARTESIAN_POINT ( 'NONE',  ( 2.789999999999999147, -9.324097380959603498, 22.25075486061734864 ) ) ;
#1288 = CARTESIAN_POINT ( 'NONE',  ( -4.840010801796527318, -3.143139765844555900, -8.812499995903225525 ) ) ;
#1289 = ORIENTED_EDGE ( 'NONE', *, *, #15396, .F. ) ;
#1290 = DIRECTION ( 'NONE',  ( 1.000000000000000000, 0.000000000000000000, 0.000000000000000000 ) ) ;
#1291 = CARTESIAN_POINT ( 'NONE',  ( -4.942249507334554259, 0.2590123213421660631, -9.968749997951615427 ) ) ;
#1292 = VERTEX_POINT ( 'NONE', #3782 ) ;
#1293 = CARTESIAN_POINT ( 'NONE',  ( 7.343749997951615427, 3.846120219227923798, 3.114526743279282694 ) ) ;
#1294 = MECHANICAL_DESIGN_GEOMETRIC_PRESENTATION_REPRESENTATION (  '', ( #18875 ), #16321 ) ;
#1295 = EDGE_CURVE ( 'NONE', #5646, #11950, #19297, .T. ) ;
#1296 = CARTESIAN_POINT ( 'NONE',  ( 2.789999999999999147, 0.000000000000000000, 0.000000000000000000 ) ) ;
#1297 = CARTESIAN_POINT ( 'NONE',  ( 13.00000000000000178, 0.000000000000000000, 0.000000000000000000 ) ) ;
#1298 = CARTESIAN_POINT ( 'NONE',  ( 12.00000000000000533, 1.185096637661215757, 5.575441324182695446 ) ) ;
#1299 = ORIENTED_EDGE ( 'NONE', *, *, #2125, .F. ) ;
#1300 = CARTESIAN_POINT ( 'NONE',  ( 11.46874999795161543, 4.888101187500000222, -2.993098736590125853E-16 ) ) ;
#1301 = PRESENTATION_STYLE_ASSIGNMENT (( #3093 ) ) ;
#1302 = DIRECTION ( 'NONE',  ( -1.000000000000000000, 0.000000000000000000, -0.000000000000000000 ) ) ;
#1303 = EDGE_CURVE ( 'NONE', #1215, #9544, #380, .T. ) ;
#1304 = ORIENTED_EDGE ( 'NONE', *, *, #4647, .T. ) ;
#1305 = CARTESIAN_POINT ( 'NONE',  ( 13.00000000000000000, -1.727010089215899713, -5.432074755721473025 ) ) ;
#1306 = EDGE_LOOP ( 'NONE', ( #18307, #12651, #14806, #1467 ) ) ;
#1307 = VECTOR ( 'NONE', #11955, 1000.000000000000000 ) ;
#1308 = FACE_OUTER_BOUND ( 'NONE', #10180, .T. ) ;
#1309 = CARTESIAN_POINT ( 'NONE',  ( 9.343749997951615427, 3.499494075959816541, -3.499494075959816541 ) ) ;
#1310 = DIRECTION ( 'NONE',  ( 1.000000000000000000, 0.000000000000000000, 0.000000000000000000 ) ) ;
#1311 = ADVANCED_FACE ( 'NONE', ( #2968 ), #1418, .T. ) ;
#1312 = CARTESIAN_POINT ( 'NONE',  ( 6.234374998975811266, -3.696815770993907903E-14, 5.294050593750000644 ) ) ;
#1313 = EDGE_LOOP ( 'NONE', ( #12513, #13833, #5318, #8910 ) ) ;
#1314 = CARTESIAN_POINT ( 'NONE',  ( 1.016293382781377819, -4.781284448697200595, -7.468749997951615427 ) ) ;
#1315 = CARTESIAN_POINT ( 'NONE',  ( 2.299999999999998490, 1.077689183249673761E-15, 8.800000000000023803 ) ) ;
#1316 = EDGE_LOOP ( 'NONE', ( #3437, #8697, #2402, #4230 ) ) ;
#1317 = AXIS2_PLACEMENT_3D ( 'NONE', #17345, #9757, #12746 ) ;
#1318 = AXIS2_PLACEMENT_3D ( 'NONE', #3845, #11458, #5724 ) ;
#1319 = CARTESIAN_POINT ( 'NONE',  ( -2.000000000000001776, 0.000000000000000000, 0.000000000000000000 ) ) ;
#1320 = CARTESIAN_POINT ( 'NONE',  ( -3.499494075959840078, -3.499494075959792116, -14.34374999795161543 ) ) ;
#1321 = ORIENTED_EDGE ( 'NONE', *, *, #8475, .T. ) ;
#1322 = CARTESIAN_POINT ( 'NONE',  ( -0.2590123213420971182, 4.942249507334556924, -7.968749997951616315 ) ) ;
#1323 = DIRECTION ( 'NONE',  ( 0.000000000000000000, 0.000000000000000000, 1.000000000000000000 ) ) ;
#1324 = CARTESIAN_POINT ( 'NONE',  ( 11.96874999795161365, 4.888101187500000222, 0.7741991708318884946 ) ) ;
#1325 = EDGE_CURVE ( 'NONE', #8102, #14997, #9403, .T. ) ;
#1326 = ORIENTED_EDGE ( 'NONE', *, *, #18116, .T. ) ;
#1327 = FACE_OUTER_BOUND ( 'NONE', #9120, .T. ) ;
#1328 = VERTEX_POINT ( 'NONE', #18186 ) ;
#1329 = CARTESIAN_POINT ( 'NONE',  ( 9.580134541264516912, -14.56230589874905412, 32.00000000000000000 ) ) ;
#1330 = ORIENTED_EDGE ( 'NONE', *, *, #12486, .F. ) ;
#1331 = DIRECTION ( 'NONE',  ( -1.000000000000000000, 0.000000000000000000, 0.000000000000000000 ) ) ;
#1332 = DIRECTION ( 'NONE',  ( 1.000000000000000000, 0.000000000000000000, 0.000000000000000000 ) ) ;
#1333 = CARTESIAN_POINT ( 'NONE',  ( 14.46874999795161720, 1.988169868018623720, -4.465502636338010589 ) ) ;
#1334 = VECTOR ( 'NONE', #5423, 1000.000000000000000 ) ;
#1335 = TOROIDAL_SURFACE ( 'NONE', #16348, 6.760799999999997034, 0.03079999999999879709 ) ;
#1336 = CARTESIAN_POINT ( 'NONE',  ( 2.604434404052930141, 19.17825124759803401, -17.45907811351434802 ) ) ;
#1337 = VERTEX_POINT ( 'NONE', #7457 ) ;
#1338 = CIRCLE ( 'NONE', #377, 6.735000000000022524 ) ;
#1339 = CARTESIAN_POINT ( 'NONE',  ( -34.92499999999994742, 9.184850993605147944E-16, -7.500000000000000000 ) ) ;
#1340 = CARTESIAN_POINT ( 'NONE',  ( 2.790000000000000924, 4.898587196589412829E-16, -4.000000000000000000 ) ) ;
#1341 = EDGE_CURVE ( 'NONE', #9831, #1519, #12084, .T. ) ;
#1342 = EDGE_CURVE ( 'NONE', #7744, #1107, #11879, .T. ) ;
#1343 = ORIENTED_EDGE ( 'NONE', *, *, #8950, .F. ) ;
#1344 = CARTESIAN_POINT ( 'NONE',  ( 2.647025296875021638, 4.584782303107579615, -6.234374998975811266 ) ) ;
#1345 = CARTESIAN_POINT ( 'NONE',  ( -0.000000000000000000, -8.000000000000003553, 37.99999999999999289 ) ) ;
#1346 = VERTEX_POINT ( 'NONE', #4276 ) ;
#1347 = CIRCLE ( 'NONE', #4219, 5.400000000000000355 ) ;
#1348 = DIRECTION ( 'NONE',  ( 1.000000000000000000, 0.000000000000000000, 0.000000000000000000 ) ) ;
#1349 = VECTOR ( 'NONE', #9495, 1000.000000000000000 ) ;
#1350 = CARTESIAN_POINT ( 'NONE',  ( 1.988169868018562880, -4.465502636338038123, -13.46874999795161543 ) ) ;
#1351 = ADVANCED_FACE ( 'NONE', ( #10582 ), #7915, .F. ) ;
#1352 = VECTOR ( 'NONE', #7469, 1000.000000000000114 ) ;
#1353 = LINE ( 'NONE', #7228, #12881 ) ;
#1354 = VERTEX_POINT ( 'NONE', #11782 ) ;
#1355 = DIRECTION ( 'NONE',  ( 0.000000000000000000, 0.000000000000000000, 1.000000000000000000 ) ) ;
#1356 = ORIENTED_EDGE ( 'NONE', *, *, #6888, .F. ) ;
#1357 = DIRECTION ( 'NONE',  ( -0.9327554006819565036, -0.3605098646343023461, 0.000000000000000000 ) ) ;
#1358 = CARTESIAN_POINT ( 'NONE',  ( 5.207209108562820710, -2.318398865532073305, -14.00000000000000533 ) ) ;
#1359 = DIRECTION ( 'NONE',  ( -1.000000000000000000, 0.000000000000000000, 0.000000000000000000 ) ) ;
#1360 = CIRCLE ( 'NONE', #3910, 2.524999999999995914 ) ;
#1361 = ORIENTED_EDGE ( 'NONE', *, *, #4390, .T. ) ;
#1362 = ORIENTED_EDGE ( 'NONE', *, *, #16739, .T. ) ;
#1363 = DIRECTION ( 'NONE',  ( -0.000000000000000000, -1.000000000000000000, -0.000000000000000000 ) ) ;
#1364 = CARTESIAN_POINT ( 'NONE',  ( 7.843749997951614539, 1.510506337161861445, -4.648860486681953397 ) ) ;
#1365 = EDGE_LOOP ( 'NONE', ( #19565, #9472, #1138, #3199, #3300, #7236, #9317, #15325 ) ) ;
#1366 = AXIS2_PLACEMENT_3D ( 'NONE', #9478, #15575, #1768 ) ;
#1367 = DIRECTION ( 'NONE',  ( 0.000000000000000000, 0.000000000000000000, -1.000000000000000000 ) ) ;
#1368 = ORIENTED_EDGE ( 'NONE', *, *, #5730, .T. ) ;
#1369 = CARTESIAN_POINT ( 'NONE',  ( 0.000000000000000000, 24.34211360614310848, -7.909232158574561744 ) ) ;
#1370 = AXIS2_PLACEMENT_3D ( 'NONE', #6319, #18637, #4934 ) ;
#1371 = DIRECTION ( 'NONE',  ( 9.559896011775280412E-17, -0.7806247497997995666, -0.6250000000000001110 ) ) ;
#1372 = PRODUCT_RELATED_PRODUCT_CATEGORY ( 'part', '', ( #1243 ) ) ;
#1373 = ORIENTED_EDGE ( 'NONE', *, *, #17144, .T. ) ;
#1374 = CIRCLE ( 'NONE', #3610, 1.000000000000000888 ) ;
#1375 = COLOUR_RGB ( '', 0.31764706, 0.68627451, 0.89019608) ;
#1376 = ADVANCED_FACE ( 'NONE', ( #4178 ), #8880, .F. ) ;
#1377 = DIRECTION ( 'NONE',  ( 0.000000000000000000, 0.000000000000000000, 1.000000000000000000 ) ) ;
#1378 = DIRECTION ( 'NONE',  ( 1.000000000000000000, -0.000000000000000000, -0.000000000000000000 ) ) ;
#1379 = DIRECTION ( 'NONE',  ( 0.000000000000000000, 0.000000000000000000, 1.000000000000000000 ) ) ;
#1380 = ADVANCED_FACE ( 'NONE', ( #10775 ), #779, .T. ) ;
#1381 = VERTEX_POINT ( 'NONE', #7657 ) ;
#1382 = DIRECTION ( 'NONE',  ( 0.000000000000000000, 0.000000000000000000, 1.000000000000000000 ) ) ;
#1383 = CARTESIAN_POINT ( 'NONE',  ( 17.11901729331276556, 5.562305898749055011, -32.00000000000000000 ) ) ;
#1384 = ORIENTED_EDGE ( 'NONE', *, *, #5542, .T. ) ;
#1385 = CYLINDRICAL_SURFACE ( 'NONE', #1537, 2.524999999999995914 ) ;
#1386 = FACE_BOUND ( 'NONE', #8709, .T. ) ;
#1387 = AXIS2_PLACEMENT_3D ( 'NONE', #13826, #11927, #6109 ) ;
#1388 = PRODUCT_DEFINITION_CONTEXT ( 'detailed design', #10473, 'design' ) ;
#1389 = CARTESIAN_POINT ( 'NONE',  ( -5.700000000000000178, 0.5990941410143899581, -9.668198987696271729 ) ) ;
#1390 = AXIS2_PLACEMENT_3D ( 'NONE', #11103, #17206, #15704 ) ;
#1391 = EDGE_CURVE ( 'NONE', #11279, #5905, #4283, .T. ) ;
#1392 = CARTESIAN_POINT ( 'NONE',  ( 4.465502636338025688, -1.988169868018592412, -14.84374999795161543 ) ) ;
#1393 = CARTESIAN_POINT ( 'NONE',  ( -5.387740456496206143, 2.068159791354259092, -11.81249999590322552 ) ) ;
#1394 = ORIENTED_EDGE ( 'NONE', *, *, #7977, .T. ) ;
#1395 = DIRECTION ( 'NONE',  ( -1.000000000000000000, -6.419766481290788001E-33, -0.000000000000000000 ) ) ;
#1396 = CARTESIAN_POINT ( 'NONE',  ( -4.233219804643852946, 2.444050593750049405, -11.46874999795161543 ) ) ;
#1397 = EDGE_CURVE ( 'NONE', #16827, #3536, #17383, .T. ) ;
#1398 = ORIENTED_EDGE ( 'NONE', *, *, #1665, .T. ) ;
#1399 = CARTESIAN_POINT ( 'NONE',  ( 11.34374999795161543, -1.773574444220757274, 4.620319390059819398 ) ) ;
#1400 = EDGE_CURVE ( 'NONE', #8532, #2993, #16980, .T. ) ;
#1401 = CARTESIAN_POINT ( 'NONE',  ( 17.28688694438834972, -7.664027248171309203, -32.00000000000000000 ) ) ;
#1402 = AXIS2_PLACEMENT_3D ( 'NONE', #15006, #10704, #16607 ) ;
#1403 = DIRECTION ( 'NONE',  ( 0.000000000000000000, 0.000000000000000000, 1.000000000000000000 ) ) ;
#1404 = CARTESIAN_POINT ( 'NONE',  ( 10.50000000000000533, 3.631840208645794821, 4.484949146646379781 ) ) ;
#1405 = ORIENTED_EDGE ( 'NONE', *, *, #10886, .T. ) ;
#1406 = CARTESIAN_POINT ( 'NONE',  ( -90.00000000000000000, 0.000000000000000000, 0.000000000000000000 ) ) ;
#1407 = CARTESIAN_POINT ( 'NONE',  ( 0.000000000000000000, 0.000000000000000000, 0.000000000000000000 ) ) ;
#1408 = DIRECTION ( 'NONE',  ( 0.000000000000000000, 0.000000000000000000, 1.000000000000000000 ) ) ;
#1409 = ORIENTED_EDGE ( 'NONE', *, *, #16598, .F. ) ;
#1410 = FACE_OUTER_BOUND ( 'NONE', #13136, .T. ) ;
#1411 = TOROIDAL_SURFACE ( 'NONE', #10087, 8.239200000000002078, 0.03079999999999868954 ) ;
#1412 = CARTESIAN_POINT ( 'NONE',  ( 2.789679245949062913, -20.70663861606260525, -12.51925356660783528 ) ) ;
#1413 = DIRECTION ( 'NONE',  ( 0.000000000000000000, 0.000000000000000000, 1.000000000000000000 ) ) ;
#1414 = EDGE_CURVE ( 'NONE', #16293, #11503, #18340, .T. ) ;
#1415 = CARTESIAN_POINT ( 'NONE',  ( 0.000000000000000000, 0.000000000000000000, 0.000000000000000000 ) ) ;
#1416 = DIRECTION ( 'NONE',  ( 1.000000000000000000, 0.000000000000000000, 0.000000000000000000 ) ) ;
#1417 = ORIENTED_EDGE ( 'NONE', *, *, #6517, .F. ) ;
#1418 = TOROIDAL_SURFACE ( 'NONE', #17709, 6.760799999999997034, 0.03079999999999879709 ) ;
#1419 = CARTESIAN_POINT ( 'NONE',  ( 2.000000000000000000, 4.999999999999998224, 37.99999999999999289 ) ) ;
#1420 = CARTESIAN_POINT ( 'NONE',  ( -2.000000000000000000, -2.000000000000002665, 41.99999999999999289 ) ) ;
#1421 = VERTEX_POINT ( 'NONE', #13774 ) ;
#1422 = AXIS2_PLACEMENT_3D ( 'NONE', #9159, #13556, #15159 ) ;
#1423 = CARTESIAN_POINT ( 'NONE',  ( -2.647025296874989664, 4.584782303107598267, -7.078124996927420476 ) ) ;
#1424 = CARTESIAN_POINT ( 'NONE',  ( 2.299999999999996270, 0.000000000000000000, 0.000000000000000000 ) ) ;
#1425 = ORIENTED_EDGE ( 'NONE', *, *, #18491, .F. ) ;
#1426 = CARTESIAN_POINT ( 'NONE',  ( 4.233219804643887585, 2.444050593749990785, -11.46874999795161543 ) ) ;
#1427 = CARTESIAN_POINT ( 'NONE',  ( 8.812499995903225525, 5.763142191869157216, -0.3020334839682480288 ) ) ;
#1428 = DIRECTION ( 'NONE',  ( -1.000000000000000000, -0.000000000000000000, -0.000000000000000000 ) ) ;
#1429 = VECTOR ( 'NONE', #11222, 1000.000000000000000 ) ;
#1430 = VERTEX_POINT ( 'NONE', #4765 ) ;
#1431 = CARTESIAN_POINT ( 'NONE',  ( 2.789999999999999147, 16.37294372382885044, -18.55949924794875017 ) ) ;
#1432 = ORIENTED_EDGE ( 'NONE', *, *, #7613, .F. ) ;
#1433 = CARTESIAN_POINT ( 'NONE',  ( -17.28688694438836393, -7.664027248171298545, 32.00000000000000000 ) ) ;
#1434 = ORIENTED_EDGE ( 'NONE', *, *, #14888, .F. ) ;
#1435 = DIRECTION ( 'NONE',  ( 1.000000000000000000, 0.000000000000000000, 0.000000000000000000 ) ) ;
#1436 = CARTESIAN_POINT ( 'NONE',  ( 16.68117051311640253, -3.372863662543048591, -32.00000000000000000 ) ) ;
#1437 = CARTESIAN_POINT ( 'NONE',  ( 0.000000000000000000, 0.000000000000000000, 0.000000000000000000 ) ) ;
#1438 = CARTESIAN_POINT ( 'NONE',  ( 8.000000000000005329, -5.668774803599153422, -0.5958122406256771697 ) ) ;
#1439 = CARTESIAN_POINT ( 'NONE',  ( 2.765633920072241292, 18.55949924794916228, -16.37294372382838148 ) ) ;
#1440 = EDGE_LOOP ( 'NONE', ( #2226, #11290, #7945, #5008 ) ) ;
#1441 = DIRECTION ( 'NONE',  ( 1.000000000000000000, 0.000000000000000000, 0.000000000000000000 ) ) ;
#1442 =( BOUNDED_CURVE ( )  B_SPLINE_CURVE ( 2, ( #19181, #2085, #15798, #15900, #795, #5474, #11300, #3588, #8495 ),
 .UNSPECIFIED., .F., .F. ) 
 B_SPLINE_CURVE_WITH_KNOTS ( ( 3, 2, 2, 2, 3 ),
 ( 0.000000000000000000, 0.04999999999999999584, 0.09999999999999999167, 0.1499999999999999944, 0.1666819079834116757 ),
 .UNSPECIFIED. ) 
 CURVE ( )  GEOMETRIC_REPRESENTATION_ITEM ( )  RATIONAL_B_SPLINE_CURVE ( ( 1.000000000000000000, 0.9876883405951377704, 1.000000000000000000, 0.9876883405951377704, 1.000000000000000000, 0.9876883405951377704, 1.000000000000000000, 0.9958923606136996787, 0.9945256517182512468 ) ) 
 REPRESENTATION_ITEM ( '' )  );
#1443 = EDGE_CURVE ( 'NONE', #3546, #9343, #18377, .T. ) ;
#1444 = CYLINDRICAL_SURFACE ( 'NONE', #5257, 7.500000000000000000 ) ;
#1445 = EDGE_LOOP ( 'NONE', ( #3057, #18115, #929, #13564 ) ) ;
#1446 = CARTESIAN_POINT ( 'NONE',  ( 13.00000000000000178, 3.849641071994447383, -3.458892414715164065 ) ) ;
#1447 = CARTESIAN_POINT ( 'NONE',  ( 2.789999999999999147, 5.535312321042718864, 23.48180575137732262 ) ) ;
#1448 = VERTEX_POINT ( 'NONE', #17551 ) ;
#1449 = VECTOR ( 'NONE', #14188, 1000.000000000000000 ) ;
#1450 = FACE_OUTER_BOUND ( 'NONE', #4388, .T. ) ;
#1452 = FACE_OUTER_BOUND ( 'NONE', #1797, .T. ) ;
#1451 = AXIS2_PLACEMENT_3D ( 'NONE', #13087, #8391, #16198 ) ;
#1453 = CARTESIAN_POINT ( 'NONE',  ( -7.671566133830872047, 15.77352024078954429, -32.00000000000000000 ) ) ;
#1454 = EDGE_LOOP ( 'NONE', ( #10584, #364, #3636 ) ) ;
#1455 = CARTESIAN_POINT ( 'NONE',  ( 2.765633920072238183, 2.336989772644269436, 24.63872515616083447 ) ) ;
#1456 = B_SPLINE_CURVE_WITH_KNOTS ( 'NONE', 3,
 ( #9561, #11157, #4748, #250 ),
 .UNSPECIFIED., .F., .F.,
 ( 4, 4 ),
 ( 0.005258214619651972732, 0.005948481662034169060 ),
 .UNSPECIFIED. ) ;
#1457 = CARTESIAN_POINT ( 'NONE',  ( 1.003445281811937204E-15, 6.667751187245561306E-16, -39.79000000000000625 ) ) ;
#1458 = CARTESIAN_POINT ( 'NONE',  ( 4.484949146646379781, 3.631840208645794821, -10.50000000000000711 ) ) ;
#1459 = DIRECTION ( 'NONE',  ( -0.000000000000000000, -0.000000000000000000, 1.000000000000000000 ) ) ;
#1460 = ORIENTED_EDGE ( 'NONE', *, *, #9951, .F. ) ;
#1461 = ADVANCED_FACE ( 'NONE', ( #3163 ), #11637, .T. ) ;
#1462 = VERTEX_POINT ( 'NONE', #14451 ) ;
#1463 = CARTESIAN_POINT ( 'NONE',  ( 0.5321745227542320489, -18.57583492944406700, -19.66801664102725056 ) ) ;
#1464 = CARTESIAN_POINT ( 'NONE',  ( 9.843749997951615427, 3.954556930911862000, -2.873153789725825469 ) ) ;
#1465 = ORIENTED_EDGE ( 'NONE', *, *, #13603, .F. ) ;
#1466 = DIRECTION ( 'NONE',  ( 0.000000000000000000, 0.000000000000000000, 1.000000000000000000 ) ) ;
#1467 = ORIENTED_EDGE ( 'NONE', *, *, #6341, .F. ) ;
#1468 = EDGE_CURVE ( 'NONE', #11673, #18486, #18038, .T. ) ;
#1469 = VECTOR ( 'NONE', #9851, 1000.000000000000114 ) ;
#1470 = DIRECTION ( 'NONE',  ( 1.000000000000000000, 0.000000000000000000, 0.000000000000000000 ) ) ;
#1471 = VERTEX_POINT ( 'NONE', #14349 ) ;
#1472 = CARTESIAN_POINT ( 'NONE',  ( 2.765633920072237295, 12.59161484032912171, 21.30679549418635688 ) ) ;
#1473 = CARTESIAN_POINT ( 'NONE',  ( 9.812499995903223748, 4.080749450109650844, -4.080749450109650844 ) ) ;
#1474 = CARTESIAN_POINT ( 'NONE',  ( 1.761396867937162769, -5.421022142882388373, -11.31249999590322375 ) ) ;
#1475 = VECTOR ( 'NONE', #7713, 1000.000000000000000 ) ;
#1476 = ORIENTED_EDGE ( 'NONE', *, *, #5448, .F. ) ;
#1477 = CARTESIAN_POINT ( 'NONE',  ( 0.02436607992776151574, -16.37294372382871188, 18.55949924794887096 ) ) ;
#1478 = SURFACE_STYLE_USAGE ( .BOTH. , #19182 ) ;
#1479 = FACE_OUTER_BOUND ( 'NONE', #9021, .T. ) ;
#1480 = ORIENTED_EDGE ( 'NONE', *, *, #19044, .F. ) ;
#1481 = EDGE_CURVE ( 'NONE', #16968, #11811, #3329, .T. ) ;
#1482 = CARTESIAN_POINT ( 'NONE',  ( 16.68117051311640253, -3.372863662543048591, -35.00000000000000000 ) ) ;
#1483 = DIRECTION ( 'NONE',  ( 0.000000000000000000, 0.000000000000000000, 1.000000000000000000 ) ) ;
#1484 = CARTESIAN_POINT ( 'NONE',  ( -16.11901729331276911, 5.562305898749051458, -32.00000000000000000 ) ) ;
#1485 = DIRECTION ( 'NONE',  ( -0.000000000000000000, 0.000000000000000000, 1.000000000000000000 ) ) ;
#1486 = ADVANCED_FACE ( 'NONE', ( #2140 ), #1085, .T. ) ;
#1487 = CARTESIAN_POINT ( 'NONE',  ( 0.7741991708318884946, 4.888101187500000222, -12.34374999795161543 ) ) ;
#1488 = ORIENTED_EDGE ( 'NONE', *, *, #5537, .T. ) ;
#1489 = CARTESIAN_POINT ( 'NONE',  ( 2.500000000000002220, 0.000000000000000000, 0.000000000000000000 ) ) ;
#1490 = ADVANCED_FACE ( 'NONE', ( #5236 ), #12273, .T. ) ;
#1491 = CARTESIAN_POINT ( 'NONE',  ( -41.99999999999999289, -5.000000000000001776, 5.000000000000000000 ) ) ;
#1492 = AXIS2_PLACEMENT_3D ( 'NONE', #4280, #1279, #14789 ) ;
#1493 = ORIENTED_EDGE ( 'NONE', *, *, #19398, .T. ) ;
#1494 = CARTESIAN_POINT ( 'NONE',  ( 12.34374999795161543, -3.114526743279282250, 3.846120219227923798 ) ) ;
#1495 = VECTOR ( 'NONE', #5397, 1000.000000000000000 ) ;
#1496 = DIRECTION ( 'NONE',  ( 0.000000000000000000, 0.000000000000000000, 1.000000000000000000 ) ) ;
#1497 = CARTESIAN_POINT ( 'NONE',  ( -2.000000000000001776, 0.000000000000000000, 0.000000000000000000 ) ) ;
#1498 = CARTESIAN_POINT ( 'NONE',  ( 12.33180101230371584, 0.5990941410143489909, 5.700000000000001066 ) ) ;
#1499 = EDGE_CURVE ( 'NONE', #871, #3717, #6504, .T. ) ;
#1500 = EDGE_CURVE ( 'NONE', #17152, #9970, #8733, .T. ) ;
#1501 = ORIENTED_EDGE ( 'NONE', *, *, #11729, .T. ) ;
#1502 = DIRECTION ( 'NONE',  ( 1.000000000000000000, 0.000000000000000000, 0.000000000000000000 ) ) ;
#1503 =( NAMED_UNIT ( * ) PLANE_ANGLE_UNIT ( ) SI_UNIT ( $, .RADIAN. ) );
#1504 = CARTESIAN_POINT ( 'NONE',  ( 1.988169868018562880, -4.465502636338038123, -13.84374999795161543 ) ) ;
#1505 = DIRECTION ( 'NONE',  ( -1.000000000000000000, 0.000000000000000000, 0.000000000000000000 ) ) ;
#1506 = ORIENTED_EDGE ( 'NONE', *, *, #7570, .F. ) ;
#1507 = CARTESIAN_POINT ( 'NONE',  ( 12.65441706489329299, -2.315350974882445456, -5.245024560144885939 ) ) ;
#1508 = VECTOR ( 'NONE', #13779, 1000.000000000000000 ) ;
#1509 = DIRECTION ( 'NONE',  ( 0.000000000000000000, 0.000000000000000000, 1.000000000000000000 ) ) ;
#1510 = EDGE_CURVE ( 'NONE', #2117, #62, #2040, .T. ) ;
#1511 = DIRECTION ( 'NONE',  ( -1.000000000000000000, 0.000000000000000000, 0.000000000000000000 ) ) ;
#1512 = AXIS2_PLACEMENT_3D ( 'NONE', #10517, #15118, #1413 ) ;
#1513 = CARTESIAN_POINT ( 'NONE',  ( 12.46874999795161543, 4.648860486681953397, 1.510506337161861223 ) ) ;
#1514 = VERTEX_POINT ( 'NONE', #9958 ) ;
#1515 = CARTESIAN_POINT ( 'NONE',  ( 13.32184790671640151, 13.12143529358541016, 32.00000000000000000 ) ) ;
#1516 = CARTESIAN_POINT ( 'NONE',  ( -15.00000000000000355, 4.215373648918918192, 3.375000000000000888 ) ) ;
#1517 = ORIENTED_EDGE ( 'NONE', *, *, #3744, .F. ) ;
#1518 = DIRECTION ( 'NONE',  ( 1.000000000000000000, 0.000000000000000000, 0.000000000000000000 ) ) ;
#1519 = VERTEX_POINT ( 'NONE', #3838 ) ;
#1520 = EDGE_CURVE ( 'NONE', #8830, #16588, #11823, .T. ) ;
#1521 = B_SPLINE_CURVE_WITH_KNOTS ( 'NONE', 3,
 ( #10115, #714, #14524, #14809, #17808, #4101 ),
 .UNSPECIFIED., .F., .F.,
 ( 4, 2, 4 ),
 ( 4.462636682232942879E-07, 0.001879885020955589887, 0.003759323778242956802 ),
 .UNSPECIFIED. ) ;
#1522 = VECTOR ( 'NONE', #13308, 1000.000000000000000 ) ;
#1523 = ADVANCED_FACE ( 'NONE', ( #1132 ), #11321, .T. ) ;
#1524 = CARTESIAN_POINT ( 'NONE',  ( -3.954556930911862000, 2.873153789725825469, -8.468749997951615427 ) ) ;
#1525 = DIRECTION ( 'NONE',  ( 0.000000000000000000, 0.000000000000000000, -1.000000000000000000 ) ) ;
#1526 = VERTEX_POINT ( 'NONE', #19141 ) ;
#1527 = CARTESIAN_POINT ( 'NONE',  ( 9.312499995903225525, 5.668774803599156975, 0.5958122406256377568 ) ) ;
#1528 = CARTESIAN_POINT ( 'NONE',  ( 13.00000000000000000, 4.333424887443004359, 2.261628166637590365 ) ) ;
#1529 = ORIENTED_EDGE ( 'NONE', *, *, #16686, .T. ) ;
#1530 = LINE ( 'NONE', #10535, #6369 ) ;
#1531 = EDGE_LOOP ( 'NONE', ( #3319, #9054, #19673, #4040, #1858 ) ) ;
#1532 = CARTESIAN_POINT ( 'NONE',  ( 5.294050593750000644, -3.696815770993907903E-14, -6.234374998975811266 ) ) ;
#1533 = VERTEX_POINT ( 'NONE', #5432 ) ;
#1534 = DIRECTION ( 'NONE',  ( -1.000000000000000000, 1.224646799147353207E-16, 0.000000000000000000 ) ) ;
#1535 = DIRECTION ( 'NONE',  ( -1.000000000000000000, -0.000000000000000000, -0.000000000000000000 ) ) ;
#1536 = CARTESIAN_POINT ( 'NONE',  ( -5.668774803599165857, -0.5958122406255588199, -9.000000000000005329 ) ) ;
#1537 = AXIS2_PLACEMENT_3D ( 'NONE', #7162, #19482, #1284 ) ;
#1538 = CARTESIAN_POINT ( 'NONE',  ( 9.968749997951615427, 4.150607464521791634, 2.695436003842732298 ) ) ;
#1539 = CIRCLE ( 'NONE', #12081, 4.200000000000000178 ) ;
#1540 = VERTEX_POINT ( 'NONE', #11540 ) ;
#1541 = LINE ( 'NONE', #8480, #8395 ) ;
#1542 =( NAMED_UNIT ( * ) SI_UNIT ( $, .STERADIAN. ) SOLID_ANGLE_UNIT ( ) );
#1543 = ORIENTED_EDGE ( 'NONE', *, *, #18666, .T. ) ;
#1544 = ADVANCED_FACE ( 'NONE', ( #8450, #2523, #8633, #17836, #13425, #8542, #11832, #10345, #17940, #6924, #14553, #4229, #7304, #19523, #5815, #13045, #846, #16049, #14741, #11636, #2335, #17645, #4035, #3935, #10054, #1028, #16155 ), #14650, .T. ) ;
#1545 = CARTESIAN_POINT ( 'NONE',  ( -16.28688694438836038, -7.664027248171298545, -35.00000000000000000 ) ) ;
#1546 = DIRECTION ( 'NONE',  ( 0.000000000000000000, 0.000000000000000000, 1.000000000000000000 ) ) ;
#1547 = AXIS2_PLACEMENT_3D ( 'NONE', #10688, #15388, #15681 ) ;
#1548 = EDGE_LOOP ( 'NONE', ( #9036, #16446, #9572, #7477, #9877, #1944, #3479, #18925 ) ) ;
#1549 = DIRECTION ( 'NONE',  ( -1.000000000000000000, -0.000000000000000000, -0.000000000000000000 ) ) ;
#1550 = CARTESIAN_POINT ( 'NONE',  ( 2.850000000000024070, 4.936344801571289409, -6.000000000000005329 ) ) ;
#1551 = ORIENTED_EDGE ( 'NONE', *, *, #5162, .T. ) ;
#1552 = CARTESIAN_POINT ( 'NONE',  ( 0.8944271909999176318, 0.000000000000000000, 6.799999999999998046 ) ) ;
#1553 = DIRECTION ( 'NONE',  ( -0.6398656649592985302, -0.7684867798512834414, 0.000000000000000000 ) ) ;
#1554 = CARTESIAN_POINT ( 'NONE',  ( -5.763142191869158992, -0.3020334839682081163, -12.50000000000000533 ) ) ;
#1555 = EDGE_CURVE ( 'NONE', #5021, #2350, #12018, .T. ) ;
#1556 = ORIENTED_EDGE ( 'NONE', *, *, #8950, .T. ) ;
#1557 =( BOUNDED_CURVE ( )  B_SPLINE_CURVE ( 2, ( #1026, #14552, #14649, #11354, #13044, #18945, #11448, #13241, #2522, #8631, #5527, #5429, #7110, #19233, #19328, #8541, #5235 ),
 .UNSPECIFIED., .F., .F. ) 
 B_SPLINE_CURVE_WITH_KNOTS ( ( 3, 2, 2, 2, 2, 2, 2, 2, 3 ),
 ( 0.000000000000000000, 0.05000000000000000971, 0.1000000000000000194, 0.1499999999999999944, 0.2000000000000000389, 0.2500000000000000000, 0.2999999999999999889, 0.3499999999999999223, 0.4000000000000000777 ),
 .UNSPECIFIED. ) 
 CURVE ( )  GEOMETRIC_REPRESENTATION_ITEM ( )  RATIONAL_B_SPLINE_CURVE ( ( 1.000000000000000000, 0.9876883405951377704, 1.000000000000000000, 0.9876883405951377704, 1.000000000000000000, 0.9876883405951377704, 1.000000000000000000, 0.9876883405951377704, 1.000000000000000000, 0.9876883405951377704, 1.000000000000000000, 0.9876883405951377704, 1.000000000000000000, 0.9876883405951377704, 1.000000000000000000, 0.9876883405951377704, 1.000000000000000000 ) ) 
 REPRESENTATION_ITEM ( '' )  );
#1558 = ORIENTED_EDGE ( 'NONE', *, *, #7927, .T. ) ;
#1559 = FACE_OUTER_BOUND ( 'NONE', #1830, .T. ) ;
#1560 = CARTESIAN_POINT ( 'NONE',  ( 2.262072661820536013, -3.461047254864073164, -26.82026385750182129 ) ) ;
#1561 = VERTEX_POINT ( 'NONE', #4622 ) ;
#1562 = CIRCLE ( 'NONE', #1886, 24.12539914357697768 ) ;
#1563 = EDGE_CURVE ( 'NONE', #2313, #18773, #2744, .T. ) ;
#1564 = ORIENTED_EDGE ( 'NONE', *, *, #9722, .T. ) ;
#1565 = FACE_OUTER_BOUND ( 'NONE', #16871, .T. ) ;
#1566 = ORIENTED_EDGE ( 'NONE', *, *, #9806, .F. ) ;
#1567 = PRODUCT_DEFINITION_FORMATION_WITH_SPECIFIED_SOURCE ( 'ANY', '', #13062, .NOT_KNOWN. ) ;
#1568 = FACE_OUTER_BOUND ( 'NONE', #7860, .T. ) ;
#1569 = CARTESIAN_POINT ( 'NONE',  ( 7.843749997951614539, 3.270778111535313837, 3.632567103900546712 ) ) ;
#1570 = CARTESIAN_POINT ( 'NONE',  ( 0.000000000000000000, 0.000000000000000000, 0.000000000000000000 ) ) ;
#1571 = CIRCLE ( 'NONE', #15323, 1.000000000000002665 ) ;
#1572 = ORIENTED_EDGE ( 'NONE', *, *, #4535, .T. ) ;
#1573 = VERTEX_POINT ( 'NONE', #8930 ) ;
#1574 = CARTESIAN_POINT ( 'NONE',  ( -6.929096493834647319, 2.870125742738179664, 12.00000000000000000 ) ) ;
#1575 = CARTESIAN_POINT ( 'NONE',  ( 0.000000000000000000, -15.04425356660774682, 20.70663861606266209 ) ) ;
#1576 = EDGE_CURVE ( 'NONE', #10781, #5905, #18332, .T. ) ;
#1577 = ORIENTED_EDGE ( 'NONE', *, *, #11824, .T. ) ;
#1578 = DIRECTION ( 'NONE',  ( -1.000000000000000000, -0.000000000000000000, -0.000000000000000000 ) ) ;
#1579 = FACE_BOUND ( 'NONE', #13672, .T. ) ;
#1580 = CONICAL_SURFACE ( 'NONE', #9252, 7.937500000000000000, 1.047197551196596521 ) ;
#1581 = CARTESIAN_POINT ( 'NONE',  ( -36.00000000000000000, 1.999999999999999112, -2.000000000000000000 ) ) ;
#1582 = DIRECTION ( 'NONE',  ( 0.000000000000000000, 0.000000000000000000, -1.000000000000000000 ) ) ;
#1583 = DIRECTION ( 'NONE',  ( 0.000000000000000000, 0.000000000000000000, -1.000000000000000000 ) ) ;
#1584 = VERTEX_POINT ( 'NONE', #4329 ) ;
#1585 = FACE_OUTER_BOUND ( 'NONE', #18734, .T. ) ;
#1586 = CARTESIAN_POINT ( 'NONE',  ( -10.00000000000000000, 0.000000000000000000, 0.000000000000000000 ) ) ;
#1587 = ORIENTED_EDGE ( 'NONE', *, *, #3578, .T. ) ;
#1588 = FACE_OUTER_BOUND ( 'NONE', #2951, .T. ) ;
#1589 = ADVANCED_FACE ( 'NONE', ( #9131 ), #7404, .F. ) ;
#1590 = CARTESIAN_POINT ( 'NONE',  ( 1.039999999999996705, -20.02152543075359503, 19.67366047555523423 ) ) ;
#1591 = AXIS2_PLACEMENT_3D ( 'NONE', #12213, #17921, #2798 ) ;
#1592 = CARTESIAN_POINT ( 'NONE',  ( 0.7589665283900990378, 3.797536611356696845, -27.31260702007171304 ) ) ;
#1593 = CARTESIAN_POINT ( 'NONE',  ( 6.500000000000005329, 5.387740456496234565, -2.068159791354182708 ) ) ;
#1594 = EDGE_CURVE ( 'NONE', #15562, #8927, #9328, .T. ) ;
#1595 = EDGE_LOOP ( 'NONE', ( #18905, #4122 ) ) ;
#1596 = CARTESIAN_POINT ( 'NONE',  ( 8.500000000000007105, 4.080749450109650844, -4.080749450109650844 ) ) ;
#1597 =( LENGTH_UNIT ( ) NAMED_UNIT ( * ) SI_UNIT ( .MILLI., .METRE. ) );
#1598 = CARTESIAN_POINT ( 'NONE',  ( 9.000000000000001776, 1.102182119232617911E-15, -35.00000000000000000 ) ) ;
#1599 = CARTESIAN_POINT ( 'NONE',  ( -10.00000000000000000, 0.000000000000000000, 0.000000000000000000 ) ) ;
#1600 = ORIENTED_EDGE ( 'NONE', *, *, #19608, .F. ) ;
#1601 = CARTESIAN_POINT ( 'NONE',  ( 2.765633920072235963, -24.63872515616080960, -2.336989772644527008 ) ) ;
#1602 = DIRECTION ( 'NONE',  ( 1.000000000000000000, 0.000000000000000000, 0.000000000000000000 ) ) ;
#1603 = DIRECTION ( 'NONE',  ( 0.7071067811865489050, 8.659560562354915602E-17, 0.7071067811865462405 ) ) ;
#1604 = CARTESIAN_POINT ( 'NONE',  ( -12.32184790671639085, 13.12143529358541549, 35.00000000000000000 ) ) ;
#1605 = ORIENTED_EDGE ( 'NONE', *, *, #17370, .F. ) ;
#1606 = DIRECTION ( 'NONE',  ( -1.000000000000000000, 0.000000000000000000, -0.000000000000000000 ) ) ;
#1607 = AXIS2_PLACEMENT_3D ( 'NONE', #3039, #16766, #18257 ) ;
#1608 = CARTESIAN_POINT ( 'NONE',  ( 2.789999999999999147, 5.456805104201435164, -23.69843731927162978 ) ) ;
#1609 = VECTOR ( 'NONE', #17718, 1000.000000000000000 ) ;
#1610 = ORIENTED_EDGE ( 'NONE', *, *, #13748, .T. ) ;
#1611 = CARTESIAN_POINT ( 'NONE',  ( 9.968749997951617203, -4.409619785863921670, 2.246813503491803310 ) ) ;
#1612 = DIRECTION ( 'NONE',  ( -1.000000000000000000, -0.000000000000000000, -0.000000000000000000 ) ) ;
#1613 = ORIENTED_EDGE ( 'NONE', *, *, #5813, .F. ) ;
#1614 = PRODUCT_DEFINITION ( 'UNKNOWN', '', #18501, #2773 ) ;
#1615 = CARTESIAN_POINT ( 'NONE',  ( -3.954556930911862000, 2.873153789725825469, -8.843749997951615427 ) ) ;
#1616 = CARTESIAN_POINT ( 'NONE',  ( 1.749999999999998002, -4.147968289691086774, -27.76164181293056288 ) ) ;
#1617 = VERTEX_POINT ( 'NONE', #13630 ) ;
#1618 = CIRCLE ( 'NONE', #5123, 28.06981291497571007 ) ;
#1619 = CARTESIAN_POINT ( 'NONE',  ( 2.789999999999999147, -20.70663861606282197, 15.04425356660753188 ) ) ;
#1620 = CARTESIAN_POINT ( 'NONE',  ( 10.96874999795161720, 4.888101187500000222, -0.7741991708318890497 ) ) ;
#1621 = ADVANCED_FACE ( 'NONE', ( #15433 ), #13529, .T. ) ;
#1622 = ORIENTED_EDGE ( 'NONE', *, *, #5804, .T. ) ;
#1623 = DIRECTION ( 'NONE',  ( 7.654042494670959086E-17, 0.6250000000000002220, 0.7806247497997996776 ) ) ;
#1624 = ORIENTED_EDGE ( 'NONE', *, *, #12199, .F. ) ;
#1625 = ADVANCED_FACE ( 'NONE', ( #19631 ), #6208, .T. ) ;
#1626 = CARTESIAN_POINT ( 'NONE',  ( 0.000000000000000000, 24.04302995059966364, -1.991882183130399664 ) ) ;
#1627 = EDGE_LOOP ( 'NONE', ( #9838, #19624, #19392, #9842, #6600, #1252 ) ) ;
#1628 = DIRECTION ( 'NONE',  ( 0.000000000000000000, 0.000000000000000000, 1.000000000000000000 ) ) ;
#1629 = FACE_OUTER_BOUND ( 'NONE', #12937, .T. ) ;
#1630 = DIRECTION ( 'NONE',  ( -1.000000000000000000, 0.000000000000000000, 0.000000000000000000 ) ) ;
#1631 = CARTESIAN_POINT ( 'NONE',  ( 11.96874999795161365, 1.773574444220725299, 4.620319390059829168 ) ) ;
#1632 = EDGE_CURVE ( 'NONE', #7691, #8343, #10533, .T. ) ;
#1633 = ORIENTED_EDGE ( 'NONE', *, *, #14674, .F. ) ;
#1634 = DIRECTION ( 'NONE',  ( 0.000000000000000000, 1.000000000000000000, -1.224646799147353207E-16 ) ) ;
#1635 = AXIS2_PLACEMENT_3D ( 'NONE', #789, #10263, #5642 ) ;
#1636 = LINE ( 'NONE', #9245, #19000 ) ;
#1637 = ADVANCED_FACE ( 'NONE', ( #16633 ), #13567, .T. ) ;
#1638 = APPLICATION_CONTEXT ( 'automotive_design' ) ;
#1639 = ORIENTED_EDGE ( 'NONE', *, *, #6877, .T. ) ;
#1640 = ADVANCED_FACE ( 'NONE', ( #3219, #15338 ), #18427, .T. ) ;
#1641 = LINE ( 'NONE', #9249, #4189 ) ;
#1642 = CARTESIAN_POINT ( 'NONE',  ( 2.255998204157473097, -17.85806462366060288, 32.00000000000000000 ) ) ;
#1643 = ORIENTED_EDGE ( 'NONE', *, *, #12286, .T. ) ;
#1644 = LINE ( 'NONE', #14046, #6665 ) ;
#1645 = CARTESIAN_POINT ( 'NONE',  ( 9.343749997951615427, -1.280903732194386579, -4.780397808154273953 ) ) ;
#1646 = LINE ( 'NONE', #14324, #4574 ) ;
#1647 = ORIENTED_EDGE ( 'NONE', *, *, #11077, .T. ) ;
#1648 = DIRECTION ( 'NONE',  ( 0.000000000000000000, 0.000000000000000000, -1.000000000000000000 ) ) ;
#1649 = VECTOR ( 'NONE', #1909, 1000.000000000000000 ) ;
#1650 = ORIENTED_EDGE ( 'NONE', *, *, #6270, .T. ) ;
#1651 = PRODUCT_CONTEXT ( 'NONE', #13526, 'mechanical' ) ;
#1652 = CIRCLE ( 'NONE', #3245, 8.265000000000021885 ) ;
#1653 = CARTESIAN_POINT ( 'NONE',  ( -5.387740456496247887, -2.068159791354146293, -11.50000000000000355 ) ) ;
#1654 = CARTESIAN_POINT ( 'NONE',  ( -5.700000000000000178, -2.180340287075187351E-16, -13.97977757194593273 ) ) ;
#1655 = CIRCLE ( 'NONE', #5170, 1.000000000000002442 ) ;
#1656 = EDGE_LOOP ( 'NONE', ( #14226, #10077, #1425, #11923 ) ) ;
#1657 = EDGE_LOOP ( 'NONE', ( #2120, #15431 ) ) ;
#1658 = DIRECTION ( 'NONE',  ( 0.9773501006361904331, 2.591706245282795403E-17, 0.2116288751244229938 ) ) ;
#1659 = EDGE_LOOP ( 'NONE', ( #3254, #3461 ) ) ;
#1660 = EDGE_CURVE ( 'NONE', #5242, #16351, #10502, .T. ) ;
#1661 = CARTESIAN_POINT ( 'NONE',  ( 2.789999999999999147, 19.64056340710875048, 14.55412442567624609 ) ) ;
#1662 = ADVANCED_FACE ( 'NONE', ( #15826, #15725 ), #2016, .F. ) ;
#1663 = VECTOR ( 'NONE', #13188, 1000.000000000000000 ) ;
#1664 = EDGE_LOOP ( 'NONE', ( #2409, #12739, #5086, #102 ) ) ;
#1665 = EDGE_CURVE ( 'NONE', #18575, #9272, #2209, .T. ) ;
#1666 = AXIS2_PLACEMENT_3D ( 'NONE', #16616, #18123, #1117 ) ;
#1667 = COLOUR_RGB ( '', 0.66274510, 0.83137255, 0.94901961) ;
#1668 = CARTESIAN_POINT ( 'NONE',  ( -5.626241948324210540, -16.73597674598852336, -32.00000000000000000 ) ) ;
#1669 = CARTESIAN_POINT ( 'NONE',  ( 13.00000000000000178, -0.7793280607714923036, -4.825575716215948496 ) ) ;
#1670 =( BOUNDED_CURVE ( )  B_SPLINE_CURVE ( 2, ( #7922, #19032, #5323, #12936, #2509, #11720, #1012, #17925, #7193, #4117, #6811, #19128, #8717, #14824, #17727, #7095, #1119 ),
 .UNSPECIFIED., .F., .F. ) 
 B_SPLINE_CURVE_WITH_KNOTS ( ( 3, 2, 2, 2, 2, 2, 2, 2, 3 ),
 ( 0.000000000000000000, 0.05000000000000000971, 0.1000000000000000194, 0.1499999999999999944, 0.2000000000000000389, 0.2500000000000000000, 0.2999999999999999889, 0.3499999999999999223, 0.4000000000000000777 ),
 .UNSPECIFIED. ) 
 CURVE ( )  GEOMETRIC_REPRESENTATION_ITEM ( )  RATIONAL_B_SPLINE_CURVE ( ( 1.000000000000000000, 0.9876883405951377704, 1.000000000000000000, 0.9876883405951377704, 1.000000000000000000, 0.9876883405951377704, 1.000000000000000000, 0.9876883405951377704, 1.000000000000000000, 0.9876883405951377704, 1.000000000000000000, 0.9876883405951377704, 1.000000000000000000, 0.9876883405951377704, 1.000000000000000000, 0.9876883405951377704, 1.000000000000000000 ) ) 
 REPRESENTATION_ITEM ( '' )  );
#1671 = CARTESIAN_POINT ( 'NONE',  ( -7.922038997698610785E-14, 18.34439787333529992, -15.96555658743743145 ) ) ;
#1672 = ORIENTED_EDGE ( 'NONE', *, *, #1563, .T. ) ;
#1673 = ORIENTED_EDGE ( 'NONE', *, *, #1481, .F. ) ;
#1674 = EDGE_CURVE ( 'NONE', #11007, #11676, #8466, .T. ) ;
#1675 = CARTESIAN_POINT ( 'NONE',  ( 0.000000000000000000, 0.000000000000000000, -29.00000000000000000 ) ) ;
#1676 = SHAPE_REPRESENTATION_RELATIONSHIP ( 'NONE' , 'NONE' ,  #12077, #3271 ) ;
#1677 = ORIENTED_EDGE ( 'NONE', *, *, #5606, .T. ) ;
#1678 = ORIENTED_EDGE ( 'NONE', *, *, #6386, .F. ) ;
#1679 = LINE ( 'NONE', #3474, #4102 ) ;
#1680 = AXIS2_PLACEMENT_3D ( 'NONE', #11781, #7250, #1377 ) ;
#1681 = FACE_BOUND ( 'NONE', #14139, .T. ) ;
#1682 = CIRCLE ( 'NONE', #12866, 28.06981291497571007 ) ;
#1683 = DIRECTION ( 'NONE',  ( 1.000000000000000000, -0.000000000000000000, -0.000000000000000000 ) ) ;
#1684 = AXIS2_PLACEMENT_3D ( 'NONE', #370, #11478, #6555 ) ;
#1685 = DIRECTION ( 'NONE',  ( -1.000000000000000000, -6.419766481290786633E-33, 0.000000000000000000 ) ) ;
#1686 = CARTESIAN_POINT ( 'NONE',  ( -1.988169868018530906, 4.465502636338051445, -13.84374999795161543 ) ) ;
#1687 = ORIENTED_EDGE ( 'NONE', *, *, #14904, .F. ) ;
#1688 = CARTESIAN_POINT ( 'NONE',  ( 2.765633920072239516, -24.15498966839958683, -5.391175441198872598 ) ) ;
#1689 = TOROIDAL_SURFACE ( 'NONE', #18618, 4.200000000000000178, 0.1999999999999998723 ) ;
#1690 = CARTESIAN_POINT ( 'NONE',  ( -14.86923836996421144, -11.47363181547641275, -32.00000000000000000 ) ) ;
#1691 = ORIENTED_EDGE ( 'NONE', *, *, #3954, .F. ) ;
#1692 = DIRECTION ( 'NONE',  ( 0.4330127018922284576, 0.7499999999999961142, 0.4999999999999977240 ) ) ;
#1693 = ADVANCED_FACE ( 'NONE', ( #11331 ), #17129, .F. ) ;
#1694 = CARTESIAN_POINT ( 'NONE',  ( 7.937500000000000000, 3.841717848563049209, -0.4950406553165793144 ) ) ;
#1695 = CIRCLE ( 'NONE', #2008, 8.073750000000021743 ) ;
#1696 = CARTESIAN_POINT ( 'NONE',  ( -5.668774803599165857, -0.5958122406255588199, -10.31249999590322552 ) ) ;
#1697 = CYLINDRICAL_SURFACE ( 'NONE', #17693, 1.000000000000005995 ) ;
#1698 = ORIENTED_EDGE ( 'NONE', *, *, #8157, .F. ) ;
#1699 = B_SPLINE_CURVE_WITH_KNOTS ( 'NONE', 3,
 ( #4812, #17021, #3311, #14707 ),
 .UNSPECIFIED., .F., .F.,
 ( 4, 4 ),
 ( 2.135345996334758909E-07, 0.0006888010880211141137 ),
 .UNSPECIFIED. ) ;
#1700 = AXIS2_PLACEMENT_3D ( 'NONE', #5124, #546, #6518 ) ;
#1701 = DIRECTION ( 'NONE',  ( 0.000000000000000000, 0.000000000000000000, -1.000000000000000000 ) ) ;
#1702 = CARTESIAN_POINT ( 'NONE',  ( 1.749999999999998002, 27.76164181293051669, 4.147968289691386090 ) ) ;
#1703 = CIRCLE ( 'NONE', #18636, 1.000000000000000888 ) ;
#1704 = DIRECTION ( 'NONE',  ( 1.000000000000000000, 0.000000000000000000, 0.000000000000000000 ) ) ;
#1705 = VERTEX_POINT ( 'NONE', #6698 ) ;
#1706 = DIRECTION ( 'NONE',  ( 0.000000000000000000, 0.000000000000000000, 1.000000000000000000 ) ) ;
#1707 = DIRECTION ( 'NONE',  ( 0.000000000000000000, 0.000000000000000000, 1.000000000000000000 ) ) ;
#1708 = CARTESIAN_POINT ( 'NONE',  ( 1.493657965219485462, -5.574407415329169169, -13.50000000000000533 ) ) ;
#1709 = DIRECTION ( 'NONE',  ( -1.000000000000000000, -0.000000000000000000, -0.000000000000000000 ) ) ;
#1710 = EDGE_CURVE ( 'NONE', #7772, #12395, #17396, .T. ) ;
#1711 = ORIENTED_EDGE ( 'NONE', *, *, #1341, .T. ) ;
#1712 = CARTESIAN_POINT ( 'NONE',  ( 0.7589665089996505687, 12.05173163741758380, -24.80232951178364686 ) ) ;
#1713 = CIRCLE ( 'NONE', #6789, 10.00000000000000000 ) ;
#1714 = CARTESIAN_POINT ( 'NONE',  ( -3.954556930911862000, 2.873153789725825469, -8.843749997951615427 ) ) ;
#1715 = ORIENTED_EDGE ( 'NONE', *, *, #15941, .T. ) ;
#1716 = DIRECTION ( 'NONE',  ( -1.000000000000000000, 1.224646799147353207E-16, 0.000000000000000000 ) ) ;
#1717 = CARTESIAN_POINT ( 'NONE',  ( 2.789999999999999147, 2.680914349914567470E-13, -25.59481291497571220 ) ) ;
#1718 = ORIENTED_EDGE ( 'NONE', *, *, #4065, .T. ) ;
#1719 = ADVANCED_FACE ( 'NONE', ( #2114, #8217 ), #17429, .F. ) ;
#1720 = VECTOR ( 'NONE', #1790, 1000.000000000000000 ) ;
#1721 = LINE ( 'NONE', #13417, #11250 ) ;
#1722 = CARTESIAN_POINT ( 'NONE',  ( 13.00000000000000000, 5.567819778318904511, 1.220402768007685657 ) ) ;
#1723 = VERTEX_POINT ( 'NONE', #15530 ) ;
#1724 = DIRECTION ( 'NONE',  ( 0.000000000000000000, 0.000000000000000000, 1.000000000000000000 ) ) ;
#1725 = DIRECTION ( 'NONE',  ( 1.000000000000000000, 0.000000000000000000, 0.000000000000000000 ) ) ;
#1726 = VERTEX_POINT ( 'NONE', #1818 ) ;
#1727 = DIRECTION ( 'NONE',  ( -1.000000000000000000, 0.000000000000000000, 0.000000000000000000 ) ) ;
#1728 = EDGE_LOOP ( 'NONE', ( #2809, #13632, #15230, #15114 ) ) ;
#1729 = DIRECTION ( 'NONE',  ( 0.000000000000000000, 1.374038396813314756E-15, -1.000000000000000000 ) ) ;
#1730 = VERTEX_POINT ( 'NONE', #14025 ) ;
#1731 = DIRECTION ( 'NONE',  ( -0.000000000000000000, -0.000000000000000000, 1.000000000000000000 ) ) ;
#1732 = DIRECTION ( 'NONE',  ( 0.000000000000000000, 0.000000000000000000, 1.000000000000000000 ) ) ;
#1733 = EDGE_CURVE ( 'NONE', #12398, #5418, #9835, .T. ) ;
#1734 = CARTESIAN_POINT ( 'NONE',  ( -5.209999999999999964, 0.000000000000000000, 0.000000000000000000 ) ) ;
#1735 = PRODUCT_RELATED_PRODUCT_CATEGORY ( 'part', '', ( #15935 ) ) ;
#1736 = CARTESIAN_POINT ( 'NONE',  ( 13.00000000000000000, 0.2080849974989116558, 4.883670121236158401 ) ) ;
#1737 = ORIENTED_EDGE ( 'NONE', *, *, #18205, .F. ) ;
#1738 = FACE_OUTER_BOUND ( 'NONE', #12469, .T. ) ;
#1739 = ADVANCED_FACE ( 'NONE', ( #12823 ), #317, .T. ) ;
#1740 = EDGE_CURVE ( 'NONE', #17455, #569, #11970, .T. ) ;
#1741 = VERTEX_POINT ( 'NONE', #12628 ) ;
#1742 = AXIS2_PLACEMENT_3D ( 'NONE', #4699, #16913, #13607 ) ;
#1743 = DIRECTION ( 'NONE',  ( -1.000000000000000000, -0.000000000000000000, -0.000000000000000000 ) ) ;
#1744 = LINE ( 'NONE', #1345, #15759 ) ;
#1745 = ORIENTED_EDGE ( 'NONE', *, *, #18107, .T. ) ;
#1746 = DIRECTION ( 'NONE',  ( 0.000000000000000000, 0.000000000000000000, 1.000000000000000000 ) ) ;
#1747 = CARTESIAN_POINT ( 'NONE',  ( 11.81249999590322552, 2.068159791354259092, -5.387740456496206143 ) ) ;
#1748 = EDGE_LOOP ( 'NONE', ( #16255, #14164, #9476, #19113 ) ) ;
#1749 = ADVANCED_FACE ( 'NONE', ( #15925 ), #2683, .T. ) ;
#1750 = DIRECTION ( 'NONE',  ( 0.000000000000000000, 0.000000000000000000, 1.000000000000000000 ) ) ;
#1751 = PRESENTATION_LAYER_ASSIGNMENT (  '', '', ( #150 ) ) ;
#1752 = VERTEX_POINT ( 'NONE', #12726 ) ;
#1753 = SHAPE_DEFINITION_REPRESENTATION ( #11783, #7967 ) ;
#1754 = LINE ( 'NONE', #13958, #6782 ) ;
#1755 = CARTESIAN_POINT ( 'NONE',  ( 12.84374999795161543, 1.016293382781411792, 4.781284448697194378 ) ) ;
#1756 = VERTEX_POINT ( 'NONE', #18718 ) ;
#1757 = ORIENTED_EDGE ( 'NONE', *, *, #3055, .F. ) ;
#1758 = CARTESIAN_POINT ( 'NONE',  ( -5.209999999999999964, 0.000000000000000000, 0.000000000000000000 ) ) ;
#1759 = CARTESIAN_POINT ( 'NONE',  ( 5.763142191869157216, 0.3020334839682480288, -13.81249999590322552 ) ) ;
#1761 = ADVANCED_FACE ( 'NONE', ( #4820 ), #10928, .T. ) ;
#1760 = EDGE_CURVE ( 'NONE', #5856, #8313, #3514, .T. ) ;
#1763 = VERTEX_POINT ( 'NONE', #9934 ) ;
#1762 = CIRCLE ( 'NONE', #19009, 9.500000000000000000 ) ;
#1764 = DIRECTION ( 'NONE',  ( 1.000000000000000000, 0.000000000000000000, 0.000000000000000000 ) ) ;
#1765 = AXIS2_PLACEMENT_3D ( 'NONE', #19492, #4393, #14903 ) ;
#1766 = ORIENTED_EDGE ( 'NONE', *, *, #12191, .T. ) ;
#1767 = DIRECTION ( 'NONE',  ( 0.000000000000000000, 0.000000000000000000, -1.000000000000000000 ) ) ;
#1768 = DIRECTION ( 'NONE',  ( 0.000000000000000000, -1.374038396813314756E-15, -1.000000000000000000 ) ) ;
#1769 = FACE_BOUND ( 'NONE', #11928, .T. ) ;
#1770 = EDGE_LOOP ( 'NONE', ( #17052, #10177, #1780, #9726 ) ) ;
#1771 = CARTESIAN_POINT ( 'NONE',  ( 2.789999999999999147, 23.48180575137737947, -5.535312321042476391 ) ) ;
#1772 = ORIENTED_EDGE ( 'NONE', *, *, #12734, .F. ) ;
#1773 = VERTEX_POINT ( 'NONE', #13219 ) ;
#1774 = CARTESIAN_POINT ( 'NONE',  ( 3.476417968967386418, 17.43449690031536292, -32.00000000000000000 ) ) ;
#1775 = AXIS2_PLACEMENT_3D ( 'NONE', #15348, #13939, #432 ) ;
#1776 = CARTESIAN_POINT ( 'NONE',  ( 12.32184790671639618, 13.12143529358541016, 35.00000000000000000 ) ) ;
#1777 = AXIS2_PLACEMENT_3D ( 'NONE', #9171, #18934, #7926 ) ;
#1778 = DIRECTION ( 'NONE',  ( 0.000000000000000000, 0.000000000000000000, 1.000000000000000000 ) ) ;
#1779 = CARTESIAN_POINT ( 'NONE',  ( -1.761396867937200739, 5.421022142882375938, -10.00000000000000533 ) ) ;
#1780 = ORIENTED_EDGE ( 'NONE', *, *, #2004, .F. ) ;
#1781 = CARTESIAN_POINT ( 'NONE',  ( 1.869200000000000195, 0.000000000000000000, 0.000000000000000000 ) ) ;
#1782 = CARTESIAN_POINT ( 'NONE',  ( 2.299999999999998934, 7.592810154713616459E-16, 6.200000000000021494 ) ) ;
#1783 = ORIENTED_EDGE ( 'NONE', *, *, #13211, .F. ) ;
#1784 = LINE ( 'NONE', #18588, #6227 ) ;
#1785 =( BOUNDED_CURVE ( )  B_SPLINE_CURVE ( 2, ( #416, #3613, #6496, #12425, #15721, #12625, #17320, #14321, #618, #6694, #3511, #17222, #11325 ),
 .UNSPECIFIED., .F., .F. ) 
 B_SPLINE_CURVE_WITH_KNOTS ( ( 3, 2, 2, 2, 2, 2, 3 ),
 ( 0.000000000000000000, 0.05000000000000000278, 0.1000000000000000056, 0.1499999999999999944, 0.2000000000000000111, 0.2500000000000000000, 0.2843253191101273170 ),
 .UNSPECIFIED. ) 
 CURVE ( )  GEOMETRIC_REPRESENTATION_ITEM ( )  RATIONAL_B_SPLINE_CURVE ( ( 1.000000000000000000, 0.9876883405951377704, 1.000000000000000000, 0.9876883405951377704, 1.000000000000000000, 0.9876883405951377704, 1.000000000000000000, 0.9876883405951377704, 1.000000000000000000, 0.9876883405951377704, 1.000000000000000000, 0.9915479672430580482, 0.9947006833465674713 ) ) 
 REPRESENTATION_ITEM ( '' )  );
#1786 = CARTESIAN_POINT ( 'NONE',  ( 9.843749997951615427, -4.465502636338009701, -1.988169868018624609 ) ) ;
#1787 = AXIS2_PLACEMENT_3D ( 'NONE', #3934, #10053, #936 ) ;
#1788 = AXIS2_PLACEMENT_3D ( 'NONE', #612, #14017, #9523 ) ;
#1789 = LINE ( 'NONE', #17293, #13177 ) ;
#1790 = DIRECTION ( 'NONE',  ( 0.000000000000000000, 0.000000000000000000, 1.000000000000000000 ) ) ;
#1791 = CARTESIAN_POINT ( 'NONE',  ( -4.611396867937224364, -3.350375938067065906, -14.00000000000000533 ) ) ;
#1792 = ORIENTED_EDGE ( 'NONE', *, *, #3339, .F. ) ;
#1793 = DIRECTION ( 'NONE',  ( -1.000000000000000000, -0.000000000000000000, -0.000000000000000000 ) ) ;
#1794 =( NAMED_UNIT ( * ) SI_UNIT ( $, .STERADIAN. ) SOLID_ANGLE_UNIT ( ) );
#1795 = CARTESIAN_POINT ( 'NONE',  ( 2.000000000000001776, 0.000000000000000000, -6.799999999999998934 ) ) ;
#1796 = DIRECTION ( 'NONE',  ( -1.000000000000000000, 0.000000000000000000, 0.000000000000000000 ) ) ;
#1797 = EDGE_LOOP ( 'NONE', ( #9983, #2137, #1209, #7611, #6830, #5049, #16780 ) ) ;
#1798 = DIRECTION ( 'NONE',  ( 0.000000000000000000, 0.000000000000000000, 1.000000000000000000 ) ) ;
#1799 = CARTESIAN_POINT ( 'NONE',  ( 0.000000000000000000, 0.000000000000000000, -35.00000000000000000 ) ) ;
#1800 = CARTESIAN_POINT ( 'NONE',  ( 9.000000000000005329, 5.207209108562820710, 2.318398865532074193 ) ) ;
#1801 = ADVANCED_FACE ( 'NONE', ( #5502 ), #2308, .T. ) ;
#1802 = CARTESIAN_POINT ( 'NONE',  ( 0.000000000000000000, 20.62201879784932856, -12.52067188844328705 ) ) ;
#1803 = VERTEX_POINT ( 'NONE', #6800 ) ;
#1804 = DIRECTION ( 'NONE',  ( 0.000000000000000000, 0.000000000000000000, 1.000000000000000000 ) ) ;
#1805 = CIRCLE ( 'NONE', #9819, 1.000000000000002665 ) ;
#1806 = CARTESIAN_POINT ( 'NONE',  ( -39.64101615137757761, -1.650388831904890594E-13, 41.99999999999999289 ) ) ;
#1807 = AXIS2_PLACEMENT_3D ( 'NONE', #8972, #16484, #19568 ) ;
#1808 = EDGE_LOOP ( 'NONE', ( #15620, #13680, #16181, #1384 ) ) ;
#1809 = CARTESIAN_POINT ( 'NONE',  ( 11.46874999795161543, -4.888101187500000222, -3.383411828340740850E-14 ) ) ;
#1810 = FACE_OUTER_BOUND ( 'NONE', #1196, .T. ) ;
#1811 = ORIENTED_EDGE ( 'NONE', *, *, #15845, .F. ) ;
#1812 = DIRECTION ( 'NONE',  ( 0.000000000000000000, 0.000000000000000000, 1.000000000000000000 ) ) ;
#1813 = EDGE_CURVE ( 'NONE', #6546, #2248, #12933, .T. ) ;
#1814 = DIRECTION ( 'NONE',  ( -0.000000000000000000, -0.000000000000000000, 1.000000000000000000 ) ) ;
#1815 = EDGE_LOOP ( 'NONE', ( #19167, #8420, #70, #12884 ) ) ;
#1816 = AXIS2_PLACEMENT_3D ( 'NONE', #1532, #10443, #7619 ) ;
#1817 = CARTESIAN_POINT ( 'NONE',  ( 2.789999999999999147, 15.74360496233408213, -18.28042085475260592 ) ) ;
#1818 = CARTESIAN_POINT ( 'NONE',  ( 1.749999999999998002, -12.96210679857767367, -24.89775460606847091 ) ) ;
#1819 = AXIS2_PLACEMENT_3D ( 'NONE', #11106, #3500, #6289 ) ;
#1820 = VECTOR ( 'NONE', #5810, 1000.000000000000000 ) ;
#1821 = ORIENTED_EDGE ( 'NONE', *, *, #10236, .T. ) ;
#1822 = DIRECTION ( 'NONE',  ( -1.000000000000000000, 0.000000000000000000, 0.000000000000000000 ) ) ;
#1823 = EDGE_LOOP ( 'NONE', ( #5096, #15538, #17838, #15877 ) ) ;
#1824 = CARTESIAN_POINT ( 'NONE',  ( 5.700000000000002842, 2.725425358843983450E-16, -10.64522241986047568 ) ) ;
#1825 = EDGE_LOOP ( 'NONE', ( #3083, #7794, #8665, #12430 ) ) ;
#1826 = DIRECTION ( 'NONE',  ( 0.000000000000000000, 0.000000000000000000, 1.000000000000000000 ) ) ;
#1827 = EDGE_CURVE ( 'NONE', #15645, #7691, #1101, .T. ) ;
#1828 = DIRECTION ( 'NONE',  ( 1.000000000000000000, -0.000000000000000000, -0.000000000000000000 ) ) ;
#1829 = CYLINDRICAL_SURFACE ( 'NONE', #3376, 2.524999999999995914 ) ;
#1830 = EDGE_LOOP ( 'NONE', ( #6602, #3647, #13917, #10088, #9890, #14417 ) ) ;
#1831 = DIRECTION ( 'NONE',  ( 1.000000000000000000, 0.000000000000000000, 0.000000000000000000 ) ) ;
#1832 = DIRECTION ( 'NONE',  ( -1.000000000000000000, 0.000000000000000000, 0.000000000000000000 ) ) ;
#1833 = AXIS2_PLACEMENT_3D ( 'NONE', #2667, #13476, #5869 ) ;
#1834 = CIRCLE ( 'NONE', #5665, 2.524999999999997691 ) ;
#1835 = B_SPLINE_CURVE_WITH_KNOTS ( 'NONE', 3,
 ( #890, #11589, #7060, #8585 ),
 .UNSPECIFIED., .F., .F.,
 ( 4, 4 ),
 ( 2.034713381942717623E-07, 0.0006887909409525284563 ),
 .UNSPECIFIED. ) ;
#1836 = ORIENTED_EDGE ( 'NONE', *, *, #12753, .T. ) ;
#1837 = CARTESIAN_POINT ( 'NONE',  ( -9.000000000000001776, 0.000000000000000000, -30.00000000000000355 ) ) ;
#1838 = EDGE_CURVE ( 'NONE', #8958, #17114, #10701, .T. ) ;
#1839 = DIRECTION ( 'NONE',  ( 0.000000000000000000, 0.000000000000000000, 1.000000000000000000 ) ) ;
#1840 = EDGE_CURVE ( 'NONE', #11336, #8576, #19311, .T. ) ;
#1841 = ORIENTED_EDGE ( 'NONE', *, *, #11626, .F. ) ;
#1842 = CARTESIAN_POINT ( 'NONE',  ( 2.765633920072235519, 24.15498966839970052, -5.391175441198366336 ) ) ;
#1843 = CARTESIAN_POINT ( 'NONE',  ( -18.11901729331277267, 5.562305898749051458, 32.00000000000000000 ) ) ;
#1844 = ORIENTED_EDGE ( 'NONE', *, *, #16931, .F. ) ;
#1845 = DIRECTION ( 'NONE',  ( 0.000000000000000000, 0.000000000000000000, 1.000000000000000000 ) ) ;
#1846 = EDGE_CURVE ( 'NONE', #2546, #9696, #3288, .T. ) ;
#1847 = CIRCLE ( 'NONE', #12704, 0.9999999999999974465 ) ;
#1848 = ORIENTED_EDGE ( 'NONE', *, *, #17371, .F. ) ;
#1849 = APPLICATION_PROTOCOL_DEFINITION ( 'draft international standard', 'automotive_design', 1998, #7767 ) ;
#1850 = CARTESIAN_POINT ( 'NONE',  ( 2.765633920072238627, 12.59161484032942901, -21.30679549418617924 ) ) ;
#1851 = CIRCLE ( 'NONE', #14319, 1.000000000000004441 ) ;
#1852 = CARTESIAN_POINT ( 'NONE',  ( 8.843749997951615427, 4.861323657744407001, 0.5109457054261784537 ) ) ;
#1853 = VERTEX_POINT ( 'NONE', #14815 ) ;
#1854 = ORIENTED_EDGE ( 'NONE', *, *, #14270, .T. ) ;
#1855 = EDGE_CURVE ( 'NONE', #10657, #10470, #19632, .T. ) ;
#1856 = CARTESIAN_POINT ( 'NONE',  ( -10.58013454126452224, -14.56230589874905235, 35.00000000000000000 ) ) ;
#1857 = CARTESIAN_POINT ( 'NONE',  ( -2.500000000000001332, 6.543750000000023270, 0.000000000000000000 ) ) ;
#1858 = ORIENTED_EDGE ( 'NONE', *, *, #2864, .T. ) ;
#1859 = EDGE_CURVE ( 'NONE', #12256, #8014, #3341, .T. ) ;
#1860 = CIRCLE ( 'NONE', #15588, 5.400000000000000355 ) ;
#1861 = ORIENTED_EDGE ( 'NONE', *, *, #5100, .F. ) ;
#1862 = VECTOR ( 'NONE', #10499, 1000.000000000000000 ) ;
#1863 = EDGE_CURVE ( 'NONE', #18773, #8014, #7084, .T. ) ;
#1864 = DIRECTION ( 'NONE',  ( 0.000000000000000000, 0.000000000000000000, 1.000000000000000000 ) ) ;
#1865 = DIRECTION ( 'NONE',  ( -0.000000000000000000, 0.000000000000000000, 1.000000000000000000 ) ) ;
#1866 = PLANE ( 'NONE',  #10369 ) ;
#1867 = ORIENTED_EDGE ( 'NONE', *, *, #12851, .F. ) ;
#1868 = DIRECTION ( 'NONE',  ( 1.000000000000000000, 0.000000000000000000, 0.000000000000000000 ) ) ;
#1869 = CARTESIAN_POINT ( 'NONE',  ( 0.000000000000000000, 0.000000000000000000, 0.000000000000000000 ) ) ;
#1870 = ORIENTED_EDGE ( 'NONE', *, *, #7757, .T. ) ;
#1871 = ORIENTED_EDGE ( 'NONE', *, *, #12830, .T. ) ;
#1872 = CARTESIAN_POINT ( 'NONE',  ( 0.006931038682727013421, -21.08061549536624568, 12.53626894672821201 ) ) ;
#1873 = CIRCLE ( 'NONE', #1231, 0.03079999999999923077 ) ;
#1874 = CARTESIAN_POINT ( 'NONE',  ( -3.143139765844656708, -4.840010801796461593, -10.81249999590322375 ) ) ;
#1875 = CARTESIAN_POINT ( 'NONE',  ( 0.000000000000000000, 0.000000000000000000, 4.000000000000000000 ) ) ;
#1876 = CARTESIAN_POINT ( 'NONE',  ( 12.99999999999999467, 4.057257337410506537, -2.726922038711639740 ) ) ;
#1877 = CARTESIAN_POINT ( 'NONE',  ( -2.246813503491833508, 4.409619785863906571, -9.968749997951617203 ) ) ;
#1878 = EDGE_LOOP ( 'NONE', ( #6627, #4972, #13147, #5239, #9251 ) ) ;
#1879 = EDGE_CURVE ( 'NONE', #11367, #12759, #13883, .T. ) ;
#1880 = CARTESIAN_POINT ( 'NONE',  ( 2.718131847775120402, -24.78765742476134548, -5.344160105508965586 ) ) ;
#1881 = CARTESIAN_POINT ( 'NONE',  ( 1.039999999999997593, 0.000000000000000000, 0.000000000000000000 ) ) ;
#1882 = ORIENTED_EDGE ( 'NONE', *, *, #16897, .T. ) ;
#1883 = CARTESIAN_POINT ( 'NONE',  ( -2.647025296875054057, -4.584782303107560963, -7.078124996927420476 ) ) ;
#1884 = CARTESIAN_POINT ( 'NONE',  ( 11.34374999795161543, -3.114526743279228072, -3.846120219227966430 ) ) ;
#1885 = EDGE_CURVE ( 'NONE', #6940, #19582, #10071, .T. ) ;
#1886 = AXIS2_PLACEMENT_3D ( 'NONE', #3455, #12761, #1946 ) ;
#1887 = EDGE_CURVE ( 'NONE', #11052, #6746, #3980, .T. ) ;
#1888 = CARTESIAN_POINT ( 'NONE',  ( -3.631840208645857437, -4.484949146646330931, -7.812499995903224637 ) ) ;
#1889 = CYLINDRICAL_SURFACE ( 'NONE', #16410, 6.799999999999998046 ) ;
#1890 = ORIENTED_EDGE ( 'NONE', *, *, #9297, .F. ) ;
#1891 = CARTESIAN_POINT ( 'NONE',  ( 6.929096493834647319, 2.870125742738179664, 0.000000000000000000 ) ) ;
#1892 = DIRECTION ( 'NONE',  ( -1.000000000000000000, -6.419766481290788001E-33, -0.000000000000000000 ) ) ;
#1893 = ORIENTED_EDGE ( 'NONE', *, *, #2125, .T. ) ;
#1894 = DIRECTION ( 'NONE',  ( 1.000000000000000000, 0.000000000000000000, 0.000000000000000000 ) ) ;
#1895 = DIRECTION ( 'NONE',  ( 0.000000000000000000, 0.000000000000000000, 1.000000000000000000 ) ) ;
#1896 = CARTESIAN_POINT ( 'NONE',  ( 8.776855558857221240, 3.635492607468361559, 12.00000000000000000 ) ) ;
#1897 = LINE ( 'NONE', #4905, #5959 ) ;
#1898 = CYLINDRICAL_SURFACE ( 'NONE', #12433, 8.265000000000021885 ) ;
#1899 = VERTEX_POINT ( 'NONE', #6993 ) ;
#1900 = FACE_OUTER_BOUND ( 'NONE', #14171, .T. ) ;
#1901 = DIRECTION ( 'NONE',  ( 0.000000000000000000, 0.000000000000000000, 1.000000000000000000 ) ) ;
#1902 = ORIENTED_EDGE ( 'NONE', *, *, #2961, .T. ) ;
#1903 = DIRECTION ( 'NONE',  ( 0.000000000000000000, 0.000000000000000000, -1.000000000000000000 ) ) ;
#1904 = ADVANCED_FACE ( 'NONE', ( #19208 ), #5254, .T. ) ;
#1905 = CARTESIAN_POINT ( 'NONE',  ( -5.000000000000000000, 1.999999999999998668, 41.99999999999999289 ) ) ;
#1906 = AXIS2_PLACEMENT_3D ( 'NONE', #8292, #697, #12365 ) ;
#1907 = EDGE_LOOP ( 'NONE', ( #6125, #4723, #348, #7790 ) ) ;
#1908 = EDGE_CURVE ( 'NONE', #7839, #10504, #16759, .T. ) ;
#1909 = DIRECTION ( 'NONE',  ( 1.000000000000000000, 0.000000000000000000, 0.000000000000000000 ) ) ;
#1910 = PLANE ( 'NONE',  #12696 ) ;
#1911 = ORIENTED_EDGE ( 'NONE', *, *, #5430, .F. ) ;
#1912 = CARTESIAN_POINT ( 'NONE',  ( 0.02436607992776238310, -2.336989772644097574, -24.63872515616085224 ) ) ;
#1913 = DIRECTION ( 'NONE',  ( 0.000000000000000000, 0.000000000000000000, -1.000000000000000000 ) ) ;
#1914 = ORIENTED_EDGE ( 'NONE', *, *, #9622, .T. ) ;
#1915 = FACE_OUTER_BOUND ( 'NONE', #6557, .T. ) ;
#1916 = ORIENTED_EDGE ( 'NONE', *, *, #12572, .T. ) ;
#1917 = CARTESIAN_POINT ( 'NONE',  ( -11.00000000000000355, 3.278623949159158446, -2.625000000000002220 ) ) ;
#1918 = ORIENTED_EDGE ( 'NONE', *, *, #989, .F. ) ;
#1919 = AXIS2_PLACEMENT_3D ( 'NONE', #3428, #13935, #130 ) ;
#1920 = EDGE_CURVE ( 'NONE', #16239, #12779, #9104, .T. ) ;
#1921 = AXIS2_PLACEMENT_3D ( 'NONE', #14124, #1623, #3423 ) ;
#1922 = FACE_BOUND ( 'NONE', #11178, .T. ) ;
#1923 = CARTESIAN_POINT ( 'NONE',  ( 1.749999999999998002, 0.000000000000000000, 0.000000000000000000 ) ) ;
#1924 = DIRECTION ( 'NONE',  ( 1.000000000000000000, 0.000000000000000000, 0.000000000000000000 ) ) ;
#1925 = CARTESIAN_POINT ( 'NONE',  ( 4.861323657744411442, 0.5109457054261445919, -9.468749997951615427 ) ) ;
#1926 = ORIENTED_EDGE ( 'NONE', *, *, #3409, .T. ) ;
#1927 = CYLINDRICAL_SURFACE ( 'NONE', #15105, 13.20000000000000284 ) ;
#1928 = DIRECTION ( 'NONE',  ( -1.000000000000000000, -0.000000000000000000, -0.000000000000000000 ) ) ;
#1929 = ORIENTED_EDGE ( 'NONE', *, *, #19038, .T. ) ;
#1930 = VECTOR ( 'NONE', #15016, 1000.000000000000000 ) ;
#1931 = CARTESIAN_POINT ( 'NONE',  ( 17.96448111170888851, 1.130229351527639148, -32.00000000000000000 ) ) ;
#1932 = ADVANCED_FACE ( 'NONE', ( #18310 ), #5989, .F. ) ;
#1933 = FACE_OUTER_BOUND ( 'NONE', #16792, .T. ) ;
#1934 = CARTESIAN_POINT ( 'NONE',  ( 5.000000000000000000, 0.000000000000000000, 37.99999999999999289 ) ) ;
#1935 = ORIENTED_EDGE ( 'NONE', *, *, #10207, .F. ) ;
#1936 = FACE_OUTER_BOUND ( 'NONE', #18621, .T. ) ;
#1937 = CARTESIAN_POINT ( 'NONE',  ( 14.31249999590322552, 5.207209108562852684, -2.318398865532001363 ) ) ;
#1938 = ORIENTED_EDGE ( 'NONE', *, *, #17938, .F. ) ;
#1939 = CARTESIAN_POINT ( 'NONE',  ( -9.000000000000000000, 1.102182119232617714E-15, 29.00000000000000355 ) ) ;
#1940 = VERTEX_POINT ( 'NONE', #4494 ) ;
#1941 = SHAPE_DEFINITION_REPRESENTATION ( #10190, #6040 ) ;
#1942 = CARTESIAN_POINT ( 'NONE',  ( -3.143139765844656708, -4.840010801796461593, -9.500000000000003553 ) ) ;
#1943 = CARTESIAN_POINT ( 'NONE',  ( 12.96874999795161543, 0.2590123213420971182, 4.942249507334556924 ) ) ;
#1944 = ORIENTED_EDGE ( 'NONE', *, *, #15674, .T. ) ;
#1945 = ORIENTED_EDGE ( 'NONE', *, *, #9793, .T. ) ;
#1946 = DIRECTION ( 'NONE',  ( 0.000000000000000000, 0.000000000000000000, 1.000000000000000000 ) ) ;
#1947 = AXIS2_PLACEMENT_3D ( 'NONE', #10506, #5686, #11900 ) ;
#1948 = DIRECTION ( 'NONE',  ( -0.4999999999999947820, -0.8660254037844417052, 0.000000000000000000 ) ) ;
#1949 = EDGE_CURVE ( 'NONE', #14997, #8102, #3656, .T. ) ;
#1950 = ORIENTED_EDGE ( 'NONE', *, *, #11138, .T. ) ;
#1951 = EDGE_CURVE ( 'NONE', #12561, #2276, #10709, .T. ) ;
#1952 = ADVANCED_FACE ( 'NONE', ( #10804 ), #99, .T. ) ;
#1953 = CARTESIAN_POINT ( 'NONE',  ( -2.000000000000000888, 0.000000000000000000, -4.200000000000000178 ) ) ;
#1954 = ORIENTED_EDGE ( 'NONE', *, *, #9226, .T. ) ;
#1955 = EDGE_CURVE ( 'NONE', #6290, #5305, #9110, .T. ) ;
#1956 = EDGE_CURVE ( 'NONE', #12131, #9602, #15813, .T. ) ;
#1957 = VECTOR ( 'NONE', #15647, 1000.000000000000000 ) ;
#1958 = AXIS2_PLACEMENT_3D ( 'NONE', #3030, #7628, #1441 ) ;
#1959 = CARTESIAN_POINT ( 'NONE',  ( -5.387740456496247887, -2.068159791354146293, -11.50000000000000355 ) ) ;
#1960 = AXIS2_PLACEMENT_3D ( 'NONE', #13369, #5755, #14978 ) ;
#1961 = DIRECTION ( 'NONE',  ( -1.000000000000000000, 0.000000000000000000, 0.000000000000000000 ) ) ;
#1962 = FACE_BOUND ( 'NONE', #8956, .T. ) ;
#1963 = ORIENTED_EDGE ( 'NONE', *, *, #19516, .F. ) ;
#1964 = CARTESIAN_POINT ( 'NONE',  ( 0.000000000000000000, -24.04302995059965653, -1.991882183130557094 ) ) ;
#1965 = DIRECTION ( 'NONE',  ( 0.000000000000000000, 0.000000000000000000, 1.000000000000000000 ) ) ;
#1966 = EDGE_LOOP ( 'NONE', ( #4725, #9031 ) ) ;
#1967 = ORIENTED_EDGE ( 'NONE', *, *, #1237, .T. ) ;
#1968 = CARTESIAN_POINT ( 'NONE',  ( 0.000000000000000000, 0.000000000000000000, 0.000000000000000000 ) ) ;
#1969 = DIRECTION ( 'NONE',  ( -1.000000000000000000, -0.000000000000000000, -0.000000000000000000 ) ) ;
#1970 = VECTOR ( 'NONE', #12424, 1000.000000000000000 ) ;
#1971 = CARTESIAN_POINT ( 'NONE',  ( -2.318398865532001363, 5.207209108562852684, -14.31249999590322552 ) ) ;
#1972 = AXIS2_PLACEMENT_3D ( 'NONE', #4783, #10596, #15496 ) ;
#1973 = ORIENTED_EDGE ( 'NONE', *, *, #10065, .T. ) ;
#1974 = CARTESIAN_POINT ( 'NONE',  ( 13.34374999795161365, 4.150607464521828938, -2.695436003842674566 ) ) ;
#1975 = CIRCLE ( 'NONE', #12857, 28.06981291497571007 ) ;
#1976 = CARTESIAN_POINT ( 'NONE',  ( 0.000000000000000000, 0.000000000000000000, -30.00000000000000355 ) ) ;
#1977 = VERTEX_POINT ( 'NONE', #1598 ) ;
#1978 = CARTESIAN_POINT ( 'NONE',  ( 5.207209108562820710, -2.318398865532073305, -14.00000000000000533 ) ) ;
#1979 = ADVANCED_FACE ( 'NONE', ( #10512 ), #15111, .F. ) ;
#1980 = CONICAL_SURFACE ( 'NONE', #4223, 4.000000000000000000, 0.7853981633974458365 ) ;
#1981 = EDGE_CURVE ( 'NONE', #8201, #5965, #13802, .T. ) ;
#1982 = CARTESIAN_POINT ( 'NONE',  ( -34.92499999999994742, 0.000000000000000000, 10.00000000000000000 ) ) ;
#1983 = DIRECTION ( 'NONE',  ( 1.000000000000000000, 0.000000000000000000, 0.000000000000000000 ) ) ;
#1984 = CARTESIAN_POINT ( 'NONE',  ( 1.749999999999998002, 12.52377138324224148, 25.12109765559658570 ) ) ;
#1985 = CARTESIAN_POINT ( 'NONE',  ( -3.499494075959840078, -3.499494075959791672, -13.96874999795161365 ) ) ;
#1986 = ORIENTED_EDGE ( 'NONE', *, *, #16386, .T. ) ;
#1987 = CIRCLE ( 'NONE', #12226, 0.9999999999999974465 ) ;
#1988 = DIRECTION ( 'NONE',  ( 0.000000000000000000, 0.000000000000000000, -1.000000000000000000 ) ) ;
#1989 = LINE ( 'NONE', #13905, #16458 ) ;
#1990 = CIRCLE ( 'NONE', #3591, 1.000000000000004441 ) ;
#1991 = DIRECTION ( 'NONE',  ( -1.000000000000000000, -0.000000000000000000, -0.000000000000000000 ) ) ;
#1992 = ORIENTED_EDGE ( 'NONE', *, *, #8446, .T. ) ;
#1993 = ADVANCED_FACE ( 'NONE', ( #18405 ), #10378, .T. ) ;
#1994 = CARTESIAN_POINT ( 'NONE',  ( 2.790000000000077751, -24.22524813288760370, -2.133839912091053836 ) ) ;
#1995 = CARTESIAN_POINT ( 'NONE',  ( -2.500000000000001776, 7.592810154713614487E-16, 6.200000000000020606 ) ) ;
#1996 = CARTESIAN_POINT ( 'NONE',  ( 5.700000000000002842, 2.725425358843983450E-16, -9.332722423957255486 ) ) ;
#1997 = AXIS2_PLACEMENT_3D ( 'NONE', #6531, #3544, #49 ) ;
#1998 = DIRECTION ( 'NONE',  ( 0.000000000000000000, 0.000000000000000000, -1.000000000000000000 ) ) ;
#1999 = DIRECTION ( 'NONE',  ( 1.000000000000000000, 0.000000000000000000, 0.000000000000000000 ) ) ;
#2000 = ORIENTED_EDGE ( 'NONE', *, *, #14470, .F. ) ;
#2001 = CARTESIAN_POINT ( 'NONE',  ( 5.207209108562820710, -2.318398865532073305, -15.31249999590322552 ) ) ;
#2002 = EDGE_CURVE ( 'NONE', #17554, #17936, #16514, .T. ) ;
#2003 = DIRECTION ( 'NONE',  ( 0.000000000000000000, 0.9510565162951567508, -0.3090169943749379589 ) ) ;
#2004 = EDGE_CURVE ( 'NONE', #10647, #18235, #14855, .T. ) ;
#2005 = ORIENTED_EDGE ( 'NONE', *, *, #7729, .T. ) ;
#2006 = CARTESIAN_POINT ( 'NONE',  ( 11.00000000000000711, 2.850000000000057820, -4.936344801571268093 ) ) ;
#2007 = CARTESIAN_POINT ( 'NONE',  ( -2.000000000000001776, 0.000000000000000000, 0.000000000000000000 ) ) ;
#2008 = AXIS2_PLACEMENT_3D ( 'NONE', #3465, #6251, #18667 ) ;
#2009 = VERTEX_POINT ( 'NONE', #8907 ) ;
#2010 = AXIS2_PLACEMENT_3D ( 'NONE', #9492, #11283, #11182 ) ;
#2011 = CARTESIAN_POINT ( 'NONE',  ( 2.765633920072242180, 22.71065055754465689, -9.836394144775473691 ) ) ;
#2012 = DIRECTION ( 'NONE',  ( 1.000000000000000000, 0.000000000000000000, 0.000000000000000000 ) ) ;
#2013 = ORIENTED_EDGE ( 'NONE', *, *, #9226, .F. ) ;
#2014 = CARTESIAN_POINT ( 'NONE',  ( 2.765633920072239516, -24.15498966839958683, -5.391175441198872598 ) ) ;
#2015 = LINE ( 'NONE', #14223, #10652 ) ;
#2016 = PLANE ( 'NONE',  #16779 ) ;
#2017 = EDGE_CURVE ( 'NONE', #12768, #13068, #7816, .T. ) ;
#2018 = ORIENTED_EDGE ( 'NONE', *, *, #6435, .F. ) ;
#2019 = CARTESIAN_POINT ( 'NONE',  ( 0.000000000000000000, -24.34211360614294506, -7.909232158575071558 ) ) ;
#2020 = ORIENTED_EDGE ( 'NONE', *, *, #13795, .F. ) ;
#2021 = CARTESIAN_POINT ( 'NONE',  ( -2.000000000000001776, 0.000000000000000000, 0.000000000000000000 ) ) ;
#2022 = AXIS2_PLACEMENT_3D ( 'NONE', #11853, #5645, #11957 ) ;
#2023 = VERTEX_POINT ( 'NONE', #1203 ) ;
#2024 = DIRECTION ( 'NONE',  ( 0.000000000000000000, 0.000000000000000000, 1.000000000000000000 ) ) ;
#2025 = DIRECTION ( 'NONE',  ( 0.000000000000000000, 0.000000000000000000, -1.000000000000000000 ) ) ;
#2026 = CARTESIAN_POINT ( 'NONE',  ( 2.789999999999999147, 0.000000000000000000, 0.000000000000000000 ) ) ;
#2027 = CARTESIAN_POINT ( 'NONE',  ( 4.781284448697187273, -1.016293382781444654, -10.46874999795161720 ) ) ;
#2028 = VERTEX_POINT ( 'NONE', #13504 ) ;
#2029 = AXIS2_PLACEMENT_3D ( 'NONE', #10316, #18109, #19603 ) ;
#2030 = CARTESIAN_POINT ( 'NONE',  ( 2.789999999999999147, -7.772527002114597572, 23.17675759782038369 ) ) ;
#2031 = CARTESIAN_POINT ( 'NONE',  ( 5.207209108562820710, -2.318398865532073305, -15.31249999590322552 ) ) ;
#2032 = ORIENTED_EDGE ( 'NONE', *, *, #11621, .F. ) ;
#2033 = CYLINDRICAL_SURFACE ( 'NONE', #12562, 1.000000000000000888 ) ;
#2034 = DIRECTION ( 'NONE',  ( -0.000000000000000000, -0.000000000000000000, 1.000000000000000000 ) ) ;
#2035 = DIRECTION ( 'NONE',  ( -1.000000000000000000, -0.000000000000000000, -0.000000000000000000 ) ) ;
#2036 = ORIENTED_EDGE ( 'NONE', *, *, #17824, .T. ) ;
#2037 = DIRECTION ( 'NONE',  ( -0.000000000000000000, -1.000000000000000000, -0.000000000000000000 ) ) ;
#2038 = CARTESIAN_POINT ( 'NONE',  ( 10.81249999590322375, 0.3020334839683282979, -5.763142191869152775 ) ) ;
#2039 = CARTESIAN_POINT ( 'NONE',  ( 13.00000000000000178, -0.7156116249825553721, -4.835865888676779356 ) ) ;
#2040 = CIRCLE ( 'NONE', #131, 3.796999999999998820 ) ;
#2041 = VERTEX_POINT ( 'NONE', #19607 ) ;
#2042 = CYLINDRICAL_SURFACE ( 'NONE', #786, 2.524999999999995914 ) ;
#2043 = ORIENTED_EDGE ( 'NONE', *, *, #11534, .F. ) ;
#2044 = APPLICATION_PROTOCOL_DEFINITION ( 'draft international standard', 'automotive_design', 1998, #7370 ) ;
#2045 = DIRECTION ( 'NONE',  ( -1.000000000000000000, 1.224646799147353207E-16, 0.000000000000000000 ) ) ;
#2046 = CARTESIAN_POINT ( 'NONE',  ( 6.000000000000005329, 0.000000000000000000, 0.000000000000000000 ) ) ;
#2047 = ORIENTED_EDGE ( 'NONE', *, *, #2731, .F. ) ;
#2048 = ORIENTED_EDGE ( 'NONE', *, *, #10407, .F. ) ;
#2049 = CARTESIAN_POINT ( 'NONE',  ( 0.4386599019957485579, -23.41653927703718097, 12.93238701107298283 ) ) ;
#2050 = LINE ( 'NONE', #12570, #8235 ) ;
#2051 = EDGE_CURVE ( 'NONE', #5844, #14373, #5895, .T. ) ;
#2052 = VERTEX_POINT ( 'NONE', #9007 ) ;
#2053 = CARTESIAN_POINT ( 'NONE',  ( -4.861323657744413218, -0.5109457054261099529, -9.843749997951615427 ) ) ;
#2054 = AXIS2_PLACEMENT_3D ( 'NONE', #11449, #14251, #3640 ) ;
#2055 = ORIENTED_EDGE ( 'NONE', *, *, #1674, .T. ) ;
#2056 = AXIS2_PLACEMENT_3D ( 'NONE', #19659, #5942, #16771 ) ;
#2057 = CARTESIAN_POINT ( 'NONE',  ( 8.000000000000000000, 0.000000000000000000, 37.99999999999999289 ) ) ;
#2058 = CARTESIAN_POINT ( 'NONE',  ( 0.02436607992776455150, -22.71065055754459650, 9.836394144775621129 ) ) ;
#2059 = EDGE_CURVE ( 'NONE', #1533, #12097, #1762, .T. ) ;
#2060 = CARTESIAN_POINT ( 'NONE',  ( 13.00000000000000178, 4.400000000000000355, 0.000000000000000000 ) ) ;
#2061 = ORIENTED_EDGE ( 'NONE', *, *, #19767, .F. ) ;
#2062 = CARTESIAN_POINT ( 'NONE',  ( 1.039999999999995373, 12.96210679857822434, -24.89775460606817958 ) ) ;
#2063 = DIRECTION ( 'NONE',  ( 0.000000000000000000, 0.000000000000000000, 1.000000000000000000 ) ) ;
#2064 = VECTOR ( 'NONE', #19500, 1000.000000000000000 ) ;
#2065 = ORIENTED_EDGE ( 'NONE', *, *, #7779, .F. ) ;
#2066 = ORIENTED_EDGE ( 'NONE', *, *, #4858, .T. ) ;
#2067 = CARTESIAN_POINT ( 'NONE',  ( 2.765633920072241736, -9.836394144775550075, -22.71065055754462492 ) ) ;
#2068 = ADVANCED_BREP_SHAPE_REPRESENTATION ( '', ( #2500, #16724 ), #120 ) ;
#2069 = ADVANCED_FACE ( 'NONE', ( #15799 ), #7987, .T. ) ;
#2070 = CARTESIAN_POINT ( 'NONE',  ( 2.789999999999999147, -15.74360496233368245, -18.28042085475295409 ) ) ;
#2071 = VECTOR ( 'NONE', #13745, 1000.000000000000000 ) ;
#2072 = CARTESIAN_POINT ( 'NONE',  ( -4.080749450109650844, 4.080749450109650844, -8.500000000000007105 ) ) ;
#2073 = ORIENTED_EDGE ( 'NONE', *, *, #10828, .T. ) ;
#2074 = LINE ( 'NONE', #11085, #6439 ) ;
#2075 =( BOUNDED_CURVE ( )  B_SPLINE_CURVE ( 2, ( #3081, #19596, #10698 ),
 .UNSPECIFIED., .F., .F. ) 
 B_SPLINE_CURVE_WITH_KNOTS ( ( 3, 3 ),
 ( 0.3333180920165871863, 0.3500000000000000333 ),
 .UNSPECIFIED. ) 
 CURVE ( )  GEOMETRIC_REPRESENTATION_ITEM ( )  RATIONAL_B_SPLINE_CURVE ( ( 0.9945256517182510247, 0.9958923606136993456, 1.000000000000000000 ) ) 
 REPRESENTATION_ITEM ( '' )  );
#2076 = CARTESIAN_POINT ( 'NONE',  ( -19.00000000000000355, 4.400000000000000355, 0.000000000000000000 ) ) ;
#2077 = VERTEX_POINT ( 'NONE', #5085 ) ;
#2078 = DIRECTION ( 'NONE',  ( -1.000000000000000000, -0.000000000000000000, 0.000000000000000000 ) ) ;
#2079 = CARTESIAN_POINT ( 'NONE',  ( 9.000000000000005329, 4.611396867937201272, -3.350375938067097437 ) ) ;
#2080 = CARTESIAN_POINT ( 'NONE',  ( 2.765633920072235075, -12.59161484032896361, -21.30679549418645280 ) ) ;
#2081 = DIRECTION ( 'NONE',  ( -1.000000000000000000, -0.000000000000000000, -0.000000000000000000 ) ) ;
#2082 = EDGE_CURVE ( 'NONE', #3194, #17426, #1989, .T. ) ;
#2083 = CARTESIAN_POINT ( 'NONE',  ( 3.499494075959791672, -3.499494075959840966, -8.968749997951611874 ) ) ;
#2084 = AXIS2_PLACEMENT_3D ( 'NONE', #7784, #6179, #12691 ) ;
#2085 = CARTESIAN_POINT ( 'NONE',  ( 7.812499995903224637, 4.484949146646356688, 3.631840208645826795 ) ) ;
#2086 = PRESENTATION_STYLE_ASSIGNMENT (( #5182 ) ) ;
#2087 = DIRECTION ( 'NONE',  ( 1.000000000000000000, 0.000000000000000000, 0.000000000000000000 ) ) ;
#2088 = CIRCLE ( 'NONE', #4975, 1.000000000000002442 ) ;
#2089 = VERTEX_POINT ( 'NONE', #9508 ) ;
#2090 = CYLINDRICAL_SURFACE ( 'NONE', #6315, 13.20000000000000107 ) ;
#2091 = ADVANCED_FACE ( 'NONE', ( #17202 ), #11099, .F. ) ;
#2092 = DIRECTION ( 'NONE',  ( 0.000000000000000000, 0.000000000000000000, 1.000000000000000000 ) ) ;
#2093 = CARTESIAN_POINT ( 'NONE',  ( 5.387740456496221242, -2.068159791354221344, -11.81249999590322552 ) ) ;
#2094 = CARTESIAN_POINT ( 'NONE',  ( 10.96874999795161720, -1.773574444220757274, 4.620319390059819398 ) ) ;
#2095 = DIRECTION ( 'NONE',  ( 1.000000000000000000, 0.000000000000000000, 0.000000000000000000 ) ) ;
#2096 = VERTEX_POINT ( 'NONE', #3494 ) ;
#2097 = EDGE_CURVE ( 'NONE', #4232, #5897, #15500, .T. ) ;
#2098 = DIRECTION ( 'NONE',  ( 0.000000000000000000, 0.000000000000000000, -1.000000000000000000 ) ) ;
#2099 = CARTESIAN_POINT ( 'NONE',  ( 0.000000000000000000, 0.000000000000000000, 0.000000000000000000 ) ) ;
#2100 = ORIENTED_EDGE ( 'NONE', *, *, #7221, .T. ) ;
#2101 = CARTESIAN_POINT ( 'NONE',  ( 9.843749997951615427, -3.954556930911881985, 2.873153789725797491 ) ) ;
#2102 = CARTESIAN_POINT ( 'NONE',  ( 0.000000000000000000, 0.000000000000000000, 0.000000000000000000 ) ) ;
#2103 = CIRCLE ( 'NONE', #8817, 1.000000000000003553 ) ;
#2104 = ORIENTED_EDGE ( 'NONE', *, *, #10242, .T. ) ;
#2105 = CARTESIAN_POINT ( 'NONE',  ( 0.000000000000000000, -15.74360496233395956, 18.28042085475273026 ) ) ;
#2106 = CIRCLE ( 'NONE', #1777, 1.000000000000004441 ) ;
#2107 = EDGE_CURVE ( 'NONE', #13012, #3997, #1115, .T. ) ;
#2108 = CARTESIAN_POINT ( 'NONE',  ( 0.000000000000000000, -15.74360496233370021, -18.28042085475294698 ) ) ;
#2109 = FACE_OUTER_BOUND ( 'NONE', #2867, .T. ) ;
#2110 = VERTEX_POINT ( 'NONE', #1795 ) ;
#2111 = DIRECTION ( 'NONE',  ( -0.000000000000000000, 0.000000000000000000, 1.000000000000000000 ) ) ;
#2112 = CARTESIAN_POINT ( 'NONE',  ( -5.700000000000000178, 0.5990941410143899581, -10.98069898359949192 ) ) ;
#2113 = ADVANCED_FACE ( 'NONE', ( #4992 ), #15699, .F. ) ;
#2114 = FACE_OUTER_BOUND ( 'NONE', #7651, .T. ) ;
#2115 = VERTEX_POINT ( 'NONE', #15604 ) ;
#2116 = DIRECTION ( 'NONE',  ( 0.000000000000000000, 0.000000000000000000, -1.000000000000000000 ) ) ;
#2117 = VERTEX_POINT ( 'NONE', #8087 ) ;
#2118 = CARTESIAN_POINT ( 'NONE',  ( 0.2436698586202201144, 0.000000000000000000, 4.824999999999999289 ) ) ;
#2119 = AXIS2_PLACEMENT_3D ( 'NONE', #14323, #15924, #10119 ) ;
#2120 = ORIENTED_EDGE ( 'NONE', *, *, #16487, .T. ) ;
#2121 = CARTESIAN_POINT ( 'NONE',  ( 0.02436607992776238310, -2.336989772644097574, -24.63872515616085224 ) ) ;
#2122 = VECTOR ( 'NONE', #4317, 1000.000000000000000 ) ;
#2123 = LINE ( 'NONE', #9640, #15256 ) ;
#2124 = CARTESIAN_POINT ( 'NONE',  ( 2.789999999999999147, 14.18181402625769749, -19.91106274590499225 ) ) ;
#2125 = EDGE_CURVE ( 'NONE', #2052, #15555, #19510, .T. ) ;
#2126 = EDGE_LOOP ( 'NONE', ( #12924, #8084, #4483, #12872, #14040, #9043, #13960, #2828 ) ) ;
#2127 = FACE_BOUND ( 'NONE', #19598, .T. ) ;
#2128 = DIRECTION ( 'NONE',  ( -1.000000000000000000, -0.000000000000000000, -0.000000000000000000 ) ) ;
#2129 = ORIENTED_EDGE ( 'NONE', *, *, #10476, .T. ) ;
#2130 = ADVANCED_FACE ( 'NONE', ( #11197 ), #9711, .F. ) ;
#2131 = AXIS2_PLACEMENT_3D ( 'NONE', #17009, #14003, #293 ) ;
#2132 = CARTESIAN_POINT ( 'NONE',  ( 90.56249999999998579, 4.774285546475956322E-16, -3.796999999999998820 ) ) ;
#2133 = AXIS2_PLACEMENT_3D ( 'NONE', #1782, #487, #12397 ) ;
#2134 = CARTESIAN_POINT ( 'NONE',  ( 2.718184749312773540, 2.576941577947758688, -25.22524549359947343 ) ) ;
#2135 = CARTESIAN_POINT ( 'NONE',  ( -11.58013454126452579, -14.56230589874905235, -35.00000000000000000 ) ) ;
#2136 = EDGE_CURVE ( 'NONE', #750, #9260, #17010, .T. ) ;
#2137 = ORIENTED_EDGE ( 'NONE', *, *, #1228, .F. ) ;
#2138 = DIRECTION ( 'NONE',  ( 1.000000000000000000, -0.000000000000000000, -0.000000000000000000 ) ) ;
#2139 = PLANE ( 'NONE',  #10424 ) ;
#2140 = FACE_OUTER_BOUND ( 'NONE', #5350, .T. ) ;
#2141 = ORIENTED_EDGE ( 'NONE', *, *, #4784, .T. ) ;
#2142 = DIRECTION ( 'NONE',  ( 0.4330127018922234616, 0.7499999999999990008, 0.4999999999999978351 ) ) ;
#2143 = ORIENTED_EDGE ( 'NONE', *, *, #2952, .T. ) ;
#2144 = CARTESIAN_POINT ( 'NONE',  ( 6.468749997951615427, 4.233219804643887585, -2.444050593749990341 ) ) ;
#2145 = ORIENTED_EDGE ( 'NONE', *, *, #5100, .T. ) ;
#2146 = ORIENTED_EDGE ( 'NONE', *, *, #5730, .F. ) ;
#2147 = B_SPLINE_CURVE_WITH_KNOTS ( 'NONE', 3,
 ( #17756, #5835, #16457, #11948, #2352, #4054 ),
 .UNSPECIFIED., .F., .F.,
 ( 4, 2, 4 ),
 ( 4.462636732217463004E-07, 0.001879885066975006029, 0.003759323870276790047 ),
 .UNSPECIFIED. ) ;
#2148 = DIRECTION ( 'NONE',  ( -0.000000000000000000, -0.000000000000000000, 1.000000000000000000 ) ) ;
#2149 = CARTESIAN_POINT ( 'NONE',  ( -13.32184790671639618, 13.12143529358541549, -32.00000000000000000 ) ) ;
#2150 = AXIS2_PLACEMENT_3D ( 'NONE', #4869, #3070, #18381 ) ;
#2151 = DIRECTION ( 'NONE',  ( 0.000000000000000000, 0.000000000000000000, 1.000000000000000000 ) ) ;
#2152 = CIRCLE ( 'NONE', #17170, 5.400000000000000355 ) ;
#2153 = EDGE_LOOP ( 'NONE', ( #16857, #17540, #2215, #19662 ) ) ;
#2154 = CARTESIAN_POINT ( 'NONE',  ( -4.620319390059805187, 1.773574444220789914, -11.34374999795161543 ) ) ;
#2155 = ORIENTED_EDGE ( 'NONE', *, *, #542, .T. ) ;
#2156 = VECTOR ( 'NONE', #12013, 1000.000000000000000 ) ;
#2157 = LINE ( 'NONE', #4763, #3488 ) ;
#2158 = EDGE_CURVE ( 'NONE', #18514, #7536, #8780, .T. ) ;
#2159 = VECTOR ( 'NONE', #8743, 1000.000000000000000 ) ;
#2160 = DIRECTION ( 'NONE',  ( 1.000000000000000000, 0.000000000000000000, 0.000000000000000000 ) ) ;
#2161 = CARTESIAN_POINT ( 'NONE',  ( 0.5321745407694753460, 26.58873630738052185, 4.993157874727903511 ) ) ;
#2162 = VERTEX_POINT ( 'NONE', #1702 ) ;
#2163 = DIRECTION ( 'NONE',  ( 1.000000000000000000, 0.000000000000000000, 0.000000000000000000 ) ) ;
#2164 = DIRECTION ( 'NONE',  ( -1.000000000000000000, -0.000000000000000000, -0.000000000000000000 ) ) ;
#2165 = ORIENTED_EDGE ( 'NONE', *, *, #14812, .T. ) ;
#2166 = ORIENTED_EDGE ( 'NONE', *, *, #5206, .T. ) ;
#2167 = CARTESIAN_POINT ( 'NONE',  ( 1.799999999999999600, 0.000000000000000000, 0.000000000000000000 ) ) ;
#2168 = EDGE_CURVE ( 'NONE', #2600, #18594, #2699, .T. ) ;
#2169 = CARTESIAN_POINT ( 'NONE',  ( 12.99999999999999467, 3.985098679772364427, -2.831373229855470797 ) ) ;
#2170 = AXIS2_PLACEMENT_3D ( 'NONE', #8194, #8589, #12800 ) ;
#2171 = CARTESIAN_POINT ( 'NONE',  ( -41.99999999999999289, -1.469576158976823947E-15, 0.000000000000000000 ) ) ;
#2172 = AXIS2_PLACEMENT_3D ( 'NONE', #17140, #18931, #14133 ) ;
#2173 = ORIENTED_EDGE ( 'NONE', *, *, #13869, .T. ) ;
#2174 = CARTESIAN_POINT ( 'NONE',  ( 8.468749997951615427, -1.988169868018530462, -4.465502636338051445 ) ) ;
#2175 = CARTESIAN_POINT ( 'NONE',  ( 12.31249999590322552, 2.850000000000057820, -4.936344801571268093 ) ) ;
#2176 = ORIENTED_EDGE ( 'NONE', *, *, #16459, .F. ) ;
#2177 = CARTESIAN_POINT ( 'NONE',  ( 16.68117051311640253, -3.372863662543048591, 32.00000000000000000 ) ) ;
#2178 = DIRECTION ( 'NONE',  ( -1.000000000000000000, 0.000000000000000000, 0.000000000000000000 ) ) ;
#2179 = EDGE_CURVE ( 'NONE', #8042, #9505, #19555, .T. ) ;
#2180 = DIRECTION ( 'NONE',  ( 1.000000000000000000, 0.000000000000000000, 0.000000000000000000 ) ) ;
#2181 = CARTESIAN_POINT ( 'NONE',  ( -17.68117051311639898, -3.372863662543042818, 32.00000000000000000 ) ) ;
#2182 = CARTESIAN_POINT ( 'NONE',  ( 2.246813503491803310, -4.409619785863921670, -9.968749997951617203 ) ) ;
#2183 = PRODUCT_DEFINITION_SHAPE ( 'NONE', 'NONE',  #19798 ) ;
#2184 = CARTESIAN_POINT ( 'NONE',  ( -2.000000000000001776, 0.000000000000000000, 0.000000000000000000 ) ) ;
#2185 = FILL_AREA_STYLE ('',( #3686 ) ) ;
#2186 = CARTESIAN_POINT ( 'NONE',  ( 2.789999999999999147, 7.909232158575156824, -21.81711360614291806 ) ) ;
#2187 = ORIENTED_EDGE ( 'NONE', *, *, #6685, .F. ) ;
#2188 = CARTESIAN_POINT ( 'NONE',  ( -90.00000000000000000, 0.000000000000000000, 0.000000000000000000 ) ) ;
#2189 = CARTESIAN_POINT ( 'NONE',  ( 4.942249507334556036, -0.2590123213421313686, -10.34374999795161543 ) ) ;
#2190 =( BOUNDED_CURVE ( )  B_SPLINE_CURVE ( 2, ( #18415, #15020, #19618, #13717, #2804, #7497, #6098, #18321, #5904, #12219, #10816, #15224, #12022, #16829, #10425, #18124, #2702 ),
 .UNSPECIFIED., .F., .F. ) 
 B_SPLINE_CURVE_WITH_KNOTS ( ( 3, 2, 2, 2, 2, 2, 2, 2, 3 ),
 ( 0.000000000000000000, 0.05000000000000000971, 0.1000000000000000194, 0.1499999999999999944, 0.2000000000000000389, 0.2500000000000000000, 0.2999999999999999889, 0.3499999999999999223, 0.4000000000000000777 ),
 .UNSPECIFIED. ) 
 CURVE ( )  GEOMETRIC_REPRESENTATION_ITEM ( )  RATIONAL_B_SPLINE_CURVE ( ( 1.000000000000000000, 0.9876883405951377704, 1.000000000000000000, 0.9876883405951377704, 1.000000000000000000, 0.9876883405951377704, 1.000000000000000000, 0.9876883405951377704, 1.000000000000000000, 0.9876883405951377704, 1.000000000000000000, 0.9876883405951377704, 1.000000000000000000, 0.9876883405951377704, 1.000000000000000000, 0.9876883405951377704, 1.000000000000000000 ) ) 
 REPRESENTATION_ITEM ( '' )  );
#2191 = EDGE_LOOP ( 'NONE', ( #10278, #7435, #9899, #9170, #318, #13941 ) ) ;
#2192 = DIRECTION ( 'NONE',  ( 0.000000000000000000, 0.000000000000000000, 1.000000000000000000 ) ) ;
#2193 = CARTESIAN_POINT ( 'NONE',  ( -2.873153789725825469, 3.954556930911862000, -9.843749997951615427 ) ) ;
#2194 = EDGE_LOOP ( 'NONE', ( #16775, #7527, #12166, #10500 ) ) ;
#2195 = CARTESIAN_POINT ( 'NONE',  ( 13.84374999795161543, -3.954556930911842016, -2.873153789725852558 ) ) ;
#2196 = ADVANCED_FACE ( 'NONE', ( #18598 ), #5183, .T. ) ;
#2197 = EDGE_CURVE ( 'NONE', #3237, #9521, #3579, .T. ) ;
#2198 = LINE ( 'NONE', #6490, #3391 ) ;
#2199 = CIRCLE ( 'NONE', #17217, 1.000000000000002665 ) ;
#2200 = ORIENTED_EDGE ( 'NONE', *, *, #19713, .T. ) ;
#2201 = FACE_OUTER_BOUND ( 'NONE', #18950, .T. ) ;
#2202 = EDGE_CURVE ( 'NONE', #16599, #5161, #426, .T. ) ;
#2203 = AXIS2_PLACEMENT_3D ( 'NONE', #1159, #6042, #4550 ) ;
#2204 = DIRECTION ( 'NONE',  ( 1.000000000000000000, 0.000000000000000000, 0.000000000000000000 ) ) ;
#2205 = CARTESIAN_POINT ( 'NONE',  ( 2.790000000000079527, -15.96555658743774941, 18.34439787333500860 ) ) ;
#2206 = EDGE_LOOP ( 'NONE', ( #19649, #8022, #10736, #4136 ) ) ;
#2207 = DIRECTION ( 'NONE',  ( 0.000000000000000000, 0.000000000000000000, -1.000000000000000000 ) ) ;
#2208 = DIRECTION ( 'NONE',  ( 0.000000000000000000, 0.000000000000000000, -1.000000000000000000 ) ) ;
#2209 = LINE ( 'NONE', #18820, #15168 ) ;
#2210 = ORIENTED_EDGE ( 'NONE', *, *, #7191, .F. ) ;
#2211 = CARTESIAN_POINT ( 'NONE',  ( 6.468749997951615427, -3.413342815706642518E-14, 4.888101187500000222 ) ) ;
#2212 = ORIENTED_EDGE ( 'NONE', *, *, #16965, .T. ) ;
#2214 = CARTESIAN_POINT ( 'NONE',  ( 2.789999999999999147, -1.991882183130126549, -24.04302995059967429 ) ) ;
#2213 = AXIS2_PLACEMENT_3D ( 'NONE', #18665, #16978, #4965 ) ;
#2215 = ORIENTED_EDGE ( 'NONE', *, *, #547, .T. ) ;
#2216 = DIRECTION ( 'NONE',  ( 0.000000000000000000, 0.000000000000000000, 1.000000000000000000 ) ) ;
#2217 = DIRECTION ( 'NONE',  ( -1.000000000000000000, -0.000000000000000000, -0.000000000000000000 ) ) ;
#2218 = CARTESIAN_POINT ( 'NONE',  ( 0.000000000000000000, 0.000000000000000000, -22.00000000000000000 ) ) ;
#2219 = COLOUR_RGB ( '', 0.66274510, 0.83137255, 0.94901961) ;
#2220 = B_SPLINE_CURVE_WITH_KNOTS ( 'NONE', 3,
 ( #19778, #9190, #6071, #12186, #18292, #15295 ),
 .UNSPECIFIED., .F., .F.,
 ( 4, 2, 4 ),
 ( 4.462636732861906317E-07, 0.001879885066975067612, 0.003759323870276849028 ),
 .UNSPECIFIED. ) ;
#2221 = CARTESIAN_POINT ( 'NONE',  ( 3.632567103900546712, 3.270778111535313837, -7.468749997951615427 ) ) ;
#2222 = ORIENTED_EDGE ( 'NONE', *, *, #15682, .F. ) ;
#2223 = DIRECTION ( 'NONE',  ( -0.000000000000000000, -0.000000000000000000, 1.000000000000000000 ) ) ;
#2224 = PRODUCT_DEFINITION ( 'UNKNOWN', '', #19766, #17599 ) ;
#2225 = CARTESIAN_POINT ( 'NONE',  ( 0.000000000000000000, -20.62201879784923264, 12.52067188844344336 ) ) ;
#2226 = ORIENTED_EDGE ( 'NONE', *, *, #5115, .F. ) ;
#2227 = FACE_OUTER_BOUND ( 'NONE', #10980, .T. ) ;
#2228 = EDGE_CURVE ( 'NONE', #7268, #758, #2782, .T. ) ;
#2229 = CARTESIAN_POINT ( 'NONE',  ( 1.749999999999998002, 0.000000000000000000, 0.000000000000000000 ) ) ;
#2230 = CARTESIAN_POINT ( 'NONE',  ( 2.789999999999999147, 0.000000000000000000, 0.000000000000000000 ) ) ;
#2231 = EDGE_CURVE ( 'NONE', #11527, #16673, #17972, .T. ) ;
#2232 = ORIENTED_EDGE ( 'NONE', *, *, #11453, .T. ) ;
#2234 = CYLINDRICAL_SURFACE ( 'NONE', #8483, 6.799999999999998046 ) ;
#2233 = CIRCLE ( 'NONE', #11507, 4.762500000000000178 ) ;
#2235 = CARTESIAN_POINT ( 'NONE',  ( -1.510506337161893642, -4.648860486681943627, -12.46874999795161543 ) ) ;
#2236 = CIRCLE ( 'NONE', #5113, 2.524999999999995914 ) ;
#2237 = CARTESIAN_POINT ( 'NONE',  ( -11.00000000000000355, 4.898587196589412829E-16, 0.000000000000000000 ) ) ;
#2238 = B_SPLINE_CURVE_WITH_KNOTS ( 'NONE', 3,
 ( #2214, #2408, #13119, #728 ),
 .UNSPECIFIED., .F., .F.,
 ( 4, 4 ),
 ( 0.005258120783916825358, 0.005948386350302978416 ),
 .UNSPECIFIED. ) ;
#2239 = VERTEX_POINT ( 'NONE', #5288 ) ;
#2240 = CARTESIAN_POINT ( 'NONE',  ( -2.179313406705571952E-17, -18.34424029220099683, -15.96500990068145853 ) ) ;
#2241 = VERTEX_POINT ( 'NONE', #696 ) ;
#2242 = ITEM_DEFINED_TRANSFORMATION ( 'NONE', 'NONE', #6975,  #16724 ) ;
#2243 = CARTESIAN_POINT ( 'NONE',  ( 13.34374999795161365, -4.150607464521812062, 2.695436003842704764 ) ) ;
#2244 = CARTESIAN_POINT ( 'NONE',  ( -4.476417968967385974, 17.43449690031536292, 32.00000000000000000 ) ) ;
#2245 = EDGE_CURVE ( 'NONE', #8648, #7952, #10616, .T. ) ;
#2246 = DIRECTION ( 'NONE',  ( 0.000000000000000000, 0.000000000000000000, 1.000000000000000000 ) ) ;
#2247 = ORIENTED_EDGE ( 'NONE', *, *, #19398, .F. ) ;
#2248 = VERTEX_POINT ( 'NONE', #11493 ) ;
#2249 = CYLINDRICAL_SURFACE ( 'NONE', #12119, 28.06981291497571362 ) ;
#2250 = DIRECTION ( 'NONE',  ( 0.000000000000000000, 0.000000000000000000, -1.000000000000000000 ) ) ;
#2251 = DIRECTION ( 'NONE',  ( 0.000000000000000000, 0.000000000000000000, 1.000000000000000000 ) ) ;
#2252 = ORIENTED_EDGE ( 'NONE', *, *, #1632, .F. ) ;
#2253 = VECTOR ( 'NONE', #9311, 1000.000000000000000 ) ;
#2254 = EDGE_CURVE ( 'NONE', #18935, #12759, #1835, .T. ) ;
#2255 = VECTOR ( 'NONE', #13804, 1000.000000000000000 ) ;
#2256 = CARTESIAN_POINT ( 'NONE',  ( 2.601776144743011443, 23.64332819722380918, 10.68696068830415946 ) ) ;
#2257 = VERTEX_POINT ( 'NONE', #14602 ) ;
#2258 = CARTESIAN_POINT ( 'NONE',  ( 2.257825467309738432, 26.83036154824994313, 3.467596033028380376 ) ) ;
#2259 = DIRECTION ( 'NONE',  ( -1.000000000000000000, -0.000000000000000000, -0.000000000000000000 ) ) ;
#2260 = DIRECTION ( 'NONE',  ( 1.000000000000000000, 0.000000000000000000, 0.000000000000000000 ) ) ;
#2261 = EDGE_LOOP ( 'NONE', ( #7376, #6155, #6525, #11274, #6937 ) ) ;
#2262 = CIRCLE ( 'NONE', #9628, 0.9999999999999974465 ) ;
#2263 = CARTESIAN_POINT ( 'NONE',  ( 0.000000000000000000, 0.000000000000000000, 0.000000000000000000 ) ) ;
#2264 = VECTOR ( 'NONE', #14846, 1000.000000000000114 ) ;
#2265 = FILL_AREA_STYLE_COLOUR ( '', #1375 ) ;
#2266 = EDGE_CURVE ( 'NONE', #15965, #10636, #12899, .T. ) ;
#2267 = EDGE_LOOP ( 'NONE', ( #2927, #12405 ) ) ;
#2268 = VERTEX_POINT ( 'NONE', #2186 ) ;
#2269 = CARTESIAN_POINT ( 'NONE',  ( 18.11901729331276911, 5.562305898749055011, 32.00000000000000000 ) ) ;
#2270 = CARTESIAN_POINT ( 'NONE',  ( 17.96448111170888851, 1.130229351527639148, 35.00000000000000000 ) ) ;
#2271 = EDGE_CURVE ( 'NONE', #12858, #1448, #6969, .T. ) ;
#2272 = LINE ( 'NONE', #10179, #11685 ) ;
#2273 = EDGE_LOOP ( 'NONE', ( #10672, #6690, #8318, #4678 ) ) ;
#2274 = CARTESIAN_POINT ( 'NONE',  ( 7.968749997951616315, -2.695436003842674566, -4.150607464521828938 ) ) ;
#2275 = CARTESIAN_POINT ( 'NONE',  ( 9.843749997951615427, -0.5109457054261099529, -4.861323657744413218 ) ) ;
#2276 = VERTEX_POINT ( 'NONE', #4087 ) ;
#2277 = DIRECTION ( 'NONE',  ( -1.000000000000000000, -0.000000000000000000, -0.000000000000000000 ) ) ;
#2278 = AXIS2_PLACEMENT_3D ( 'NONE', #13838, #18436, #19734 ) ;
#2279 = CARTESIAN_POINT ( 'NONE',  ( 10.50000000000000533, 5.700000000000000178, -0.9027913098498572264 ) ) ;
#2280 = APPLICATION_CONTEXT ( 'automotive_design' ) ;
#2281 = CARTESIAN_POINT ( 'NONE',  ( 2.765633920072234631, 5.391175441198615914, 24.15498966839965078 ) ) ;
#2282 = DIRECTION ( 'NONE',  ( 1.000000000000000000, 6.419766481290786633E-33, -0.000000000000000000 ) ) ;
#2283 = CARTESIAN_POINT ( 'NONE',  ( -16.28688694438836038, -7.664027248171298545, 32.00000000000000000 ) ) ;
#2284 = DIRECTION ( 'NONE',  ( 1.000000000000000000, 0.000000000000000000, 0.000000000000000000 ) ) ;
#2285 = DIRECTION ( 'NONE',  ( 1.000000000000000000, 0.000000000000000000, 0.000000000000000000 ) ) ;
#2286 = ORIENTED_EDGE ( 'NONE', *, *, #16716, .T. ) ;
#2287 = EDGE_CURVE ( 'NONE', #18497, #9970, #14121, .T. ) ;
#2288 = DIRECTION ( 'NONE',  ( -1.000000000000000000, 0.000000000000000000, 0.000000000000000000 ) ) ;
#2289 = AXIS2_PLACEMENT_3D ( 'NONE', #6520, #8137, #11044 ) ;
#2290 = CYLINDRICAL_SURFACE ( 'NONE', #3298, 6.000000000000000000 ) ;
#2291 = AXIS2_PLACEMENT_3D ( 'NONE', #6294, #6200, #11114 ) ;
#2292 = CARTESIAN_POINT ( 'NONE',  ( 8.843749997951615427, -4.861323657744403448, -0.5109457054262123155 ) ) ;
#2293 = DIRECTION ( 'NONE',  ( 0.000000000000000000, 0.000000000000000000, 1.000000000000000000 ) ) ;
#2294 = CARTESIAN_POINT ( 'NONE',  ( 2.789999999999999147, -0.2301004812059262439, 24.44424927289185590 ) ) ;
#2295 = EDGE_CURVE ( 'NONE', #14128, #3813, #15099, .T. ) ;
#2296 = ORIENTED_EDGE ( 'NONE', *, *, #13115, .F. ) ;
#2297 = CARTESIAN_POINT ( 'NONE',  ( 12.00000000000000533, 4.235925505221192822, -3.814044456245444081 ) ) ;
#2298 = CARTESIAN_POINT ( 'NONE',  ( 2.783025336474041822, 12.53640742967753141, 21.08118142846907972 ) ) ;
#2299 = ORIENTED_EDGE ( 'NONE', *, *, #7127, .F. ) ;
#2300 =( LENGTH_UNIT ( ) NAMED_UNIT ( * ) SI_UNIT ( .MILLI., .METRE. ) );
#2301 = FACE_OUTER_BOUND ( 'NONE', #3565, .T. ) ;
#2302 = AXIS2_PLACEMENT_3D ( 'NONE', #9106, #18305, #10602 ) ;
#2303 = CIRCLE ( 'NONE', #9022, 1.000000000000002665 ) ;
#2304 = CIRCLE ( 'NONE', #13485, 10.00000000000000000 ) ;
#2305 = CARTESIAN_POINT ( 'NONE',  ( 12.00000000000000000, 0.000000000000000000, 3.593999999999999861 ) ) ;
#2306 = ORIENTED_EDGE ( 'NONE', *, *, #1555, .T. ) ;
#2307 = DIRECTION ( 'NONE',  ( 0.000000000000000000, 0.000000000000000000, 1.000000000000000000 ) ) ;
#2308 = CYLINDRICAL_SURFACE ( 'NONE', #791, 13.19999999999999929 ) ;
#2309 = CIRCLE ( 'NONE', #724, 8.073750000000021743 ) ;
#2310 = ORIENTED_EDGE ( 'NONE', *, *, #977, .T. ) ;
#2311 = EDGE_CURVE ( 'NONE', #241, #2766, #17890, .T. ) ;
#2312 = DIRECTION ( 'NONE',  ( 0.000000000000000000, 0.000000000000000000, -1.000000000000000000 ) ) ;
#2313 = VERTEX_POINT ( 'NONE', #8682 ) ;
#2314 = DIRECTION ( 'NONE',  ( 1.000000000000000000, 0.000000000000000000, 0.000000000000000000 ) ) ;
#2315 = ORIENTED_EDGE ( 'NONE', *, *, #3702, .F. ) ;
#2316 = CARTESIAN_POINT ( 'NONE',  ( 0.006974663525957706944, 21.08118142846903353, 12.53640742967760602 ) ) ;
#2317 = CARTESIAN_POINT ( 'NONE',  ( 4.080749450109649956, 4.080749450109650844, -14.81249999590322375 ) ) ;
#2318 = DIRECTION ( 'NONE',  ( 0.000000000000000000, 0.000000000000000000, 1.000000000000000000 ) ) ;
#2319 = CIRCLE ( 'NONE', #15751, 1.000000000000000000 ) ;
#2320 = STYLED_ITEM ( 'NONE', ( #4664 ), #9128 ) ;
#2321 = DIRECTION ( 'NONE',  ( 1.000000000000000000, 0.000000000000000000, -0.000000000000000000 ) ) ;
#2322 = EDGE_CURVE ( 'NONE', #1899, #15854, #8394, .T. ) ;
#2323 = EDGE_LOOP ( 'NONE', ( #8523, #233, #1361, #4923 ) ) ;
#2324 = CARTESIAN_POINT ( 'NONE',  ( 2.765633920072235519, 9.836394144776026138, -22.71065055754441531 ) ) ;
#2325 = CARTESIAN_POINT ( 'NONE',  ( 2.299999999999998490, 0.000000000000000000, 0.000000000000000000 ) ) ;
#2326 = ORIENTED_EDGE ( 'NONE', *, *, #4591, .F. ) ;
#2327 = CIRCLE ( 'NONE', #6156, 1.000000000000000888 ) ;
#2328 = AXIS2_PLACEMENT_3D ( 'NONE', #14174, #11177, #4970 ) ;
#2329 = FACE_OUTER_BOUND ( 'NONE', #1169, .T. ) ;
#2330 = CARTESIAN_POINT ( 'NONE',  ( 2.873153789725797491, -3.954556930911881985, -9.843749997951615427 ) ) ;
#2331 = EDGE_LOOP ( 'NONE', ( #171, #18959 ) ) ;
#2332 =( GEOMETRIC_REPRESENTATION_CONTEXT ( 3 ) GLOBAL_UNCERTAINTY_ASSIGNED_CONTEXT ( ( #11792 ) ) GLOBAL_UNIT_ASSIGNED_CONTEXT ( ( #9933, #11707, #16020 ) ) REPRESENTATION_CONTEXT ( 'NONE', 'WORKASPACE' ) );
#2333 = DIRECTION ( 'NONE',  ( -1.000000000000000000, -0.000000000000000000, -0.000000000000000000 ) ) ;
#2334 = CARTESIAN_POINT ( 'NONE',  ( 1.999999999999999556, -5.000000000000001776, 41.99999999999999289 ) ) ;
#2335 = FACE_BOUND ( 'NONE', #13427, .T. ) ;
#2336 = EDGE_LOOP ( 'NONE', ( #18850, #5277, #7151, #9720, #1068, #13183, #13467, #16106 ) ) ;
#2337 = ADVANCED_FACE ( 'NONE', ( #5573 ), #1980, .T. ) ;
#2338 = CARTESIAN_POINT ( 'NONE',  ( -20.63749999999999929, 6.368163355566236381E-16, 5.200000000000000178 ) ) ;
#2339 = PRODUCT_DEFINITION ( 'UNKNOWN', '', #1567, #18196 ) ;
#2340 = ORIENTED_EDGE ( 'NONE', *, *, #8723, .T. ) ;
#2341 = CIRCLE ( 'NONE', #14165, 2.524999999999996803 ) ;
#2342 = SURFACE_STYLE_FILL_AREA ( #17651 ) ;
#2343 = CARTESIAN_POINT ( 'NONE',  ( -1.799999999999999600, 0.000000000000000000, 0.000000000000000000 ) ) ;
#2344 = VECTOR ( 'NONE', #10398, 1000.000000000000000 ) ;
#2345 = CARTESIAN_POINT ( 'NONE',  ( -15.28688694438835505, -7.664027248171298545, 32.00000000000000000 ) ) ;
#2346 = ORIENTED_EDGE ( 'NONE', *, *, #14684, .T. ) ;
#2347 = DIRECTION ( 'NONE',  ( 0.000000000000000000, -1.000000000000000000, 0.000000000000000000 ) ) ;
#2348 = DIRECTION ( 'NONE',  ( 1.000000000000000000, 0.000000000000000000, 0.000000000000000000 ) ) ;
#2349 = DIRECTION ( 'NONE',  ( -0.000000000000000000, -0.000000000000000000, -1.000000000000000000 ) ) ;
#2350 = VERTEX_POINT ( 'NONE', #19088 ) ;
#2351 = ADVANCED_FACE ( 'NONE', ( #5382 ), #11684, .T. ) ;
#2352 = CARTESIAN_POINT ( 'NONE',  ( 2.718184749312773540, -2.576941577947583273, 25.22524549359949120 ) ) ;
#2353 = PRODUCT_DEFINITION_SHAPE ( 'NONE', 'NONE',  #7470 ) ;
#2354 = EDGE_LOOP ( 'NONE', ( #17229, #17352, #14279, #8703 ) ) ;
#2355 = EDGE_CURVE ( 'NONE', #298, #881, #8539, .T. ) ;
#2356 = EDGE_CURVE ( 'NONE', #15965, #6632, #7398, .T. ) ;
#2357 = PLANE ( 'NONE',  #12766 ) ;
#2358 = VERTEX_POINT ( 'NONE', #16200 ) ;
#2359 = DIRECTION ( 'NONE',  ( 1.000000000000000000, 0.000000000000000000, 0.000000000000000000 ) ) ;
#2360 = AXIS2_PLACEMENT_3D ( 'NONE', #14551, #9956, #15850 ) ;
#2361 = DIRECTION ( 'NONE',  ( 0.000000000000000000, 0.000000000000000000, 1.000000000000000000 ) ) ;
#2362 = EDGE_CURVE ( 'NONE', #8447, #1803, #2309, .T. ) ;
#2363 = SURFACE_STYLE_USAGE ( .BOTH. , #12875 ) ;
#2364 = ORIENTED_EDGE ( 'NONE', *, *, #11308, .T. ) ;
#2365 = VERTEX_POINT ( 'NONE', #9087 ) ;
#2366 = CARTESIAN_POINT ( 'NONE',  ( -4.611396867937224364, -3.350375938067065906, -15.31249999590322552 ) ) ;
#2367 = AXIS2_PLACEMENT_3D ( 'NONE', #12036, #18138, #4424 ) ;
#2368 = CARTESIAN_POINT ( 'NONE',  ( 2.765633920072239071, -16.37294372382844543, -18.55949924794910544 ) ) ;
#2369 = CARTESIAN_POINT ( 'NONE',  ( -2.849999999999988987, 4.936344801571308061, -6.000000000000005329 ) ) ;
#2370 = VERTEX_POINT ( 'NONE', #12181 ) ;
#2371 = CARTESIAN_POINT ( 'NONE',  ( 12.34374999795161543, 3.114526743279308896, -3.846120219227901593 ) ) ;
#2372 = CARTESIAN_POINT ( 'NONE',  ( 11.31249999590322375, 1.185096637661293251, -5.575441324182679459 ) ) ;
#2373 = VECTOR ( 'NONE', #13954, 1000.000000000000000 ) ;
#2374 = EDGE_LOOP ( 'NONE', ( #18650, #10854, #1844, #12183, #11255 ) ) ;
#2375 = DIRECTION ( 'NONE',  ( -1.000000000000000000, 0.000000000000000000, -0.000000000000000000 ) ) ;
#2376 = AXIS2_PLACEMENT_3D ( 'NONE', #16021, #4107, #11708 ) ;
#2377 = FACE_OUTER_BOUND ( 'NONE', #7576, .T. ) ;
#2378 = CARTESIAN_POINT ( 'NONE',  ( 4.305564957446062380, 6.679616436190405793, 4.844604941820970789E-15 ) ) ;
#2379 = DIRECTION ( 'NONE',  ( -0.000000000000000000, -0.000000000000000000, 1.000000000000000000 ) ) ;
#2380 = CARTESIAN_POINT ( 'NONE',  ( 0.000000000000000000, 0.000000000000000000, 0.000000000000000000 ) ) ;
#2381 = CARTESIAN_POINT ( 'NONE',  ( 0.006974674093432167536, 2.249040938978497994, 24.42374957165206695 ) ) ;
#2382 = DIRECTION ( 'NONE',  ( 0.000000000000000000, 0.000000000000000000, 1.000000000000000000 ) ) ;
#2383 = EDGE_LOOP ( 'NONE', ( #11428, #15343, #7208, #3839 ) ) ;
#2384 = CARTESIAN_POINT ( 'NONE',  ( 10.81249999590322375, 4.840010801796482909, 3.143139765844622957 ) ) ;
#2385 = CIRCLE ( 'NONE', #18054, 5.400000000000000355 ) ;
#2386 = DIRECTION ( 'NONE',  ( 1.000000000000000000, -0.000000000000000000, -0.000000000000000000 ) ) ;
#2387 = UNCERTAINTY_MEASURE_WITH_UNIT (LENGTH_MEASURE( 1.000000000000000082E-05 ), #7591, 'distance_accuracy_value', 'NONE');
#2388 = CARTESIAN_POINT ( 'NONE',  ( 3.632567103900546712, 3.270778111535313837, -7.843749997951614539 ) ) ;
#2389 = CARTESIAN_POINT ( 'NONE',  ( 10.34374999795161543, -4.150607464521772094, -2.695436003842760275 ) ) ;
#2390 = CARTESIAN_POINT ( 'NONE',  ( 0.1882239080259289210, -5.251266773802552024, 25.40949241676352344 ) ) ;
#2391 = CARTESIAN_POINT ( 'NONE',  ( 3.350375938067096548, 4.611396867937201272, -14.31249999590322552 ) ) ;
#2392 = ORIENTED_EDGE ( 'NONE', *, *, #6340, .F. ) ;
#2393 = CARTESIAN_POINT ( 'NONE',  ( 15.31249999590322552, -3.350375938067065906, -4.611396867937224364 ) ) ;
#2394 = CARTESIAN_POINT ( 'NONE',  ( 5.207209108562838473, 2.318398865532038666, -9.312499995903225525 ) ) ;
#2395 = ORIENTED_EDGE ( 'NONE', *, *, #2705, .T. ) ;
#2396 = LINE ( 'NONE', #3899, #482 ) ;
#2397 = CARTESIAN_POINT ( 'NONE',  ( -2.500000000000002220, 0.000000000000000000, -8.800000000000022027 ) ) ;
#2398 = VECTOR ( 'NONE', #8181, 1000.000000000000000 ) ;
#2399 = CIRCLE ( 'NONE', #12641, 1.000000000000004441 ) ;
#2400 = FACE_OUTER_BOUND ( 'NONE', #5133, .T. ) ;
#2401 = CARTESIAN_POINT ( 'NONE',  ( 2.765633920072235963, -16.37294372382871188, 18.55949924794887096 ) ) ;
#2402 = ORIENTED_EDGE ( 'NONE', *, *, #10017, .F. ) ;
#2403 = DIRECTION ( 'NONE',  ( -1.000000000000000000, 0.000000000000000000, 0.000000000000000000 ) ) ;
#2404 = CARTESIAN_POINT ( 'NONE',  ( 0.000000000000000000, 0.000000000000000000, 35.00000000000000000 ) ) ;
#2405 = EDGE_CURVE ( 'NONE', #13251, #9816, #3032, .T. ) ;
#2406 = CARTESIAN_POINT ( 'NONE',  ( 90.56249999999998579, 0.000000000000000000, 0.000000000000000000 ) ) ;
#2407 = VERTEX_POINT ( 'NONE', #8786 ) ;
#2408 = CARTESIAN_POINT ( 'NONE',  ( 2.789999999999999147, -2.133490293296841589, -24.22479935914661198 ) ) ;
#2409 = ORIENTED_EDGE ( 'NONE', *, *, #13411, .T. ) ;
#2410 = DIRECTION ( 'NONE',  ( 1.000000000000000000, 0.000000000000000000, 0.000000000000000000 ) ) ;
#2411 = CARTESIAN_POINT ( 'NONE',  ( 0.000000000000000000, 0.000000000000000000, -32.00000000000000000 ) ) ;
#2412 = DIRECTION ( 'NONE',  ( 1.000000000000000000, 0.000000000000000000, 0.000000000000000000 ) ) ;
#2413 = AXIS2_PLACEMENT_3D ( 'NONE', #11245, #7837, #4842 ) ;
#2414 = CARTESIAN_POINT ( 'NONE',  ( -17.96448111170888851, 1.130229351527647585, -32.00000000000000000 ) ) ;
#2415 = AXIS2_PLACEMENT_3D ( 'NONE', #16479, #13274, #15072 ) ;
#2416 = ORIENTED_EDGE ( 'NONE', *, *, #7238, .F. ) ;
#2417 = DIRECTION ( 'NONE',  ( 0.000000000000000000, 0.000000000000000000, 1.000000000000000000 ) ) ;
#2418 = LINE ( 'NONE', #1015, #10750 ) ;
#2419 = VERTEX_POINT ( 'NONE', #5963 ) ;
#2420 = CARTESIAN_POINT ( 'NONE',  ( 9.671566133830877376, 15.77352024078954784, -35.00000000000000000 ) ) ;
#2421 = ORIENTED_EDGE ( 'NONE', *, *, #6751, .T. ) ;
#2422 = AXIS2_PLACEMENT_3D ( 'NONE', #19522, #10438, #1323 ) ;
#2423 = CARTESIAN_POINT ( 'NONE',  ( 0.02436607992775674525, 9.836394144776026138, -22.71065055754441531 ) ) ;
#2424 = CARTESIAN_POINT ( 'NONE',  ( 0.5109457054261454800, -4.861323657744410554, -14.84374999795161543 ) ) ;
#2425 = DIRECTION ( 'NONE',  ( 1.000000000000000000, -0.000000000000000000, -0.000000000000000000 ) ) ;
#2426 = EDGE_CURVE ( 'NONE', #1337, #4347, #6604, .T. ) ;
#2427 = AXIS2_PLACEMENT_3D ( 'NONE', #2325, #8440, #13036 ) ;
#2428 = ORIENTED_EDGE ( 'NONE', *, *, #11867, .T. ) ;
#2429 = CARTESIAN_POINT ( 'NONE',  ( 2.783025342027734883, 23.92335783895644852, -5.408388659523843067 ) ) ;
#2430 = ORIENTED_EDGE ( 'NONE', *, *, #18387, .F. ) ;
#2431 = ITEM_DEFINED_TRANSFORMATION ( 'NONE', 'NONE', #12111,  #16724 ) ;
#2432 = CARTESIAN_POINT ( 'NONE',  ( 2.030753616560876829, -24.80264696524875490, -12.05220173035465336 ) ) ;
#2433 = DIRECTION ( 'NONE',  ( -1.000000000000000000, 0.000000000000000000, 0.000000000000000000 ) ) ;
#2434 = ORIENTED_EDGE ( 'NONE', *, *, #17702, .T. ) ;
#2435 = DIRECTION ( 'NONE',  ( 0.000000000000000000, 0.000000000000000000, 1.000000000000000000 ) ) ;
#2436 = CARTESIAN_POINT ( 'NONE',  ( 2.789999999999999147, 19.91106274590514147, 14.18181402625749676 ) ) ;
#2437 = CARTESIAN_POINT ( 'NONE',  ( -16.19790265903627713, 9.644882309621941374, 35.00000000000000000 ) ) ;
#2438 = ORIENTED_EDGE ( 'NONE', *, *, #6884, .T. ) ;
#2439 = CARTESIAN_POINT ( 'NONE',  ( -2.000000000000001776, 8.247996192257451316E-16, 6.735000000000022524 ) ) ;
#2440 = ADVANCED_FACE ( 'NONE', ( #1479 ), #15087, .F. ) ;
#2441 = EDGE_CURVE ( 'NONE', #8277, #15013, #7462, .T. ) ;
#2442 = ORIENTED_EDGE ( 'NONE', *, *, #14853, .T. ) ;
#2443 = ADVANCED_FACE ( 'NONE', ( #9185 ), #10293, .T. ) ;
#2444 = CARTESIAN_POINT ( 'NONE',  ( 1.749999999999998002, 27.76164181293051669, 4.147968289691386090 ) ) ;
#2445 = CARTESIAN_POINT ( 'NONE',  ( 13.00000000000000533, -4.611396867937178179, -3.350375938067128967 ) ) ;
#2446 = VERTEX_POINT ( 'NONE', #10685 ) ;
#2447 = CARTESIAN_POINT ( 'NONE',  ( -4.942249507334553371, 0.2590123213421660631, -9.968749997951617203 ) ) ;
#2448 = ADVANCED_FACE ( 'NONE', ( #1181 ), #9347, .F. ) ;
#2449 = AXIS2_PLACEMENT_3D ( 'NONE', #4135, #16247, #10249 ) ;
#2450 =( NAMED_UNIT ( * ) PLANE_ANGLE_UNIT ( ) SI_UNIT ( $, .RADIAN. ) );
#2451 = FILL_AREA_STYLE ('',( #2265 ) ) ;
#2452 = VECTOR ( 'NONE', #4478, 1000.000000000000000 ) ;
#2453 = ORIENTED_EDGE ( 'NONE', *, *, #10690, .F. ) ;
#2454 = EDGE_LOOP ( 'NONE', ( #3809, #13101, #10322, #6636 ) ) ;
#2455 = CARTESIAN_POINT ( 'NONE',  ( -4.781284448697179279, 1.016293382781477961, -10.46874999795161720 ) ) ;
#2456 = CARTESIAN_POINT ( 'NONE',  ( 9.968749997951617203, -0.2590123213421313686, 4.942249507334556036 ) ) ;
#2457 = EDGE_CURVE ( 'NONE', #18074, #5711, #13490, .T. ) ;
#2458 = CARTESIAN_POINT ( 'NONE',  ( -2.255998204157477538, -17.85806462366060288, 35.00000000000000000 ) ) ;
#2459 = ORIENTED_EDGE ( 'NONE', *, *, #10655, .T. ) ;
#2460 = DIRECTION ( 'NONE',  ( -1.000000000000000000, 0.000000000000000000, 0.000000000000000000 ) ) ;
#2461 = CARTESIAN_POINT ( 'NONE',  ( 6.843749997951615427, -4.233219804643852946, -2.444050593750049849 ) ) ;
#2462 = CIRCLE ( 'NONE', #13658, 2.524999999999996358 ) ;
#2463 = ORIENTED_EDGE ( 'NONE', *, *, #13603, .T. ) ;
#2464 = DIRECTION ( 'NONE',  ( 1.000000000000000000, 0.000000000000000000, 0.000000000000000000 ) ) ;
#2465 = EDGE_CURVE ( 'NONE', #16863, #2982, #1360, .T. ) ;
#2466 = VECTOR ( 'NONE', #3155, 1000.000000000000000 ) ;
#2467 = EDGE_CURVE ( 'NONE', #1561, #9666, #6442, .T. ) ;
#2468 = DIRECTION ( 'NONE',  ( 0.000000000000000000, 1.000000000000000000, 0.000000000000000000 ) ) ;
#2469 = LINE ( 'NONE', #8677, #7463 ) ;
#2470 = CYLINDRICAL_SURFACE ( 'NONE', #16114, 13.19999999999999929 ) ;
#2471 = ADVANCED_FACE ( 'NONE', ( #11882, #12088 ), #5766, .T. ) ;
#2472 = LINE ( 'NONE', #11984, #18118 ) ;
#2473 = CARTESIAN_POINT ( 'NONE',  ( -2.500000000000002220, 0.000000000000000000, 0.000000000000000000 ) ) ;
#2474 = ORIENTED_EDGE ( 'NONE', *, *, #10806, .T. ) ;
#2475 = SHAPE_REPRESENTATION ( 'plain washer clevis pin grade a_iso_ISO 8738 - 12', ( #16724 ), #17389 ) ;
#2476 = CARTESIAN_POINT ( 'NONE',  ( 11.31249999590322375, 4.235925505221138643, 3.814044456245502701 ) ) ;
#2477 = DIRECTION ( 'NONE',  ( 0.000000000000000000, 0.000000000000000000, 1.000000000000000000 ) ) ;
#2478 = CARTESIAN_POINT ( 'NONE',  ( 4.233219804643871598, -2.444050593750019651, -11.84374999795161365 ) ) ;
#2479 = CIRCLE ( 'NONE', #251, 30.00000000000000355 ) ;
#2480 = EDGE_CURVE ( 'NONE', #18417, #2569, #18920, .T. ) ;
#2481 = DIRECTION ( 'NONE',  ( 0.000000000000000000, 0.000000000000000000, 1.000000000000000000 ) ) ;
#2482 = CARTESIAN_POINT ( 'NONE',  ( -0.9027913098498572264, 5.699999999999999289, -11.81249999590322552 ) ) ;
#2483 = ORIENTED_EDGE ( 'NONE', *, *, #10663, .T. ) ;
#2484 = CARTESIAN_POINT ( 'NONE',  ( 2.789999999999999147, -12.52067188844365830, 20.62201879784908698 ) ) ;
#2485 = DIRECTION ( 'NONE',  ( 1.000000000000000000, 0.000000000000000000, 0.000000000000000000 ) ) ;
#2486 = EDGE_CURVE ( 'NONE', #17826, #18420, #5275, .T. ) ;
#2487 = ORIENTED_EDGE ( 'NONE', *, *, #6656, .T. ) ;
#2488 = CARTESIAN_POINT ( 'NONE',  ( 0.000000000000000000, 0.000000000000000000, -30.00000000000000355 ) ) ;
#2489 = ADVANCED_FACE ( 'NONE', ( #12287 ), #18089, .F. ) ;
#2490 = CARTESIAN_POINT ( 'NONE',  ( -2.000000000000001776, 5.388445916248354013E-16, -4.400000000000000355 ) ) ;
#2491 = AXIS2_PLACEMENT_3D ( 'NONE', #6337, #3251, #18656 ) ;
#2492 = FACE_OUTER_BOUND ( 'NONE', #17685, .T. ) ;
#2493 = CARTESIAN_POINT ( 'NONE',  ( 2.783025228907522575, 22.53337530003403799, 9.686319561461028016 ) ) ;
#2494 = ORIENTED_EDGE ( 'NONE', *, *, #10561, .T. ) ;
#2495 = B_SPLINE_CURVE_WITH_KNOTS ( 'NONE', 3,
 ( #1007, #17722, #6808, #12829, #6902, #2121 ),
 .UNSPECIFIED., .F., .F.,
 ( 4, 2, 4 ),
 ( 4.462636732861906317E-07, 0.001879885066975067178, 0.003759323870276848160 ),
 .UNSPECIFIED. ) ;
#2496 = CARTESIAN_POINT ( 'NONE',  ( 3.954556930911861112, 2.873153789725825913, -14.46874999795161720 ) ) ;
#2497 = DIRECTION ( 'NONE',  ( 0.000000000000000000, 0.000000000000000000, -1.000000000000000000 ) ) ;
#2498 = CARTESIAN_POINT ( 'NONE',  ( -3.207603742328077057E-13, 82.80384757729329692, 41.99999999999999289 ) ) ;
#2499 = ORIENTED_EDGE ( 'NONE', *, *, #3937, .F. ) ;
#2500 = MANIFOLD_SOLID_BREP ( 'Bore', #8722 ) ;
#2501 = DIRECTION ( 'NONE',  ( 0.000000000000000000, 0.000000000000000000, 1.000000000000000000 ) ) ;
#2502 = VERTEX_POINT ( 'NONE', #3471 ) ;
#2503 = CARTESIAN_POINT ( 'NONE',  ( 0.07186808533286645484, -10.24630254990532663, 23.19485392143210944 ) ) ;
#2504 = CARTESIAN_POINT ( 'NONE',  ( 2.718131914667133220, 23.19485392143227642, -10.24630254990492340 ) ) ;
#2505 = ADVANCED_FACE ( 'NONE', ( #6649 ), #11985, .F. ) ;
#2506 = PRODUCT ( 'BR-591', 'BR-591', '', ( #12456 ) ) ;
#2507 = CARTESIAN_POINT ( 'NONE',  ( 2.255998204157473097, -17.85806462366060288, 32.00000000000000000 ) ) ;
#2508 = AXIS2_PLACEMENT_3D ( 'NONE', #4240, #10254, #2629 ) ;
#2509 = CARTESIAN_POINT ( 'NONE',  ( -4.611396867937201272, 3.350375938067097437, -8.000000000000005329 ) ) ;
#2510 = EDGE_LOOP ( 'NONE', ( #7828, #1460, #3224, #15446 ) ) ;
#2511 = PLANE ( 'NONE',  #16664 ) ;
#2512 = CARTESIAN_POINT ( 'NONE',  ( 0.2436698586202201144, 0.000000000000000000, 0.000000000000000000 ) ) ;
#2513 = ADVANCED_FACE ( 'NONE', ( #15678 ), #18477, .T. ) ;
#2514 = ORIENTED_EDGE ( 'NONE', *, *, #19377, .T. ) ;
#2515 = ADVANCED_FACE ( 'NONE', ( #14276 ), #15385, .T. ) ;
#2516 = FACE_OUTER_BOUND ( 'NONE', #16831, .T. ) ;
#2517 = CARTESIAN_POINT ( 'NONE',  ( -0.5109457054261112852, 4.861323657744413218, -14.46874999795161720 ) ) ;
#2518 = AXIS2_PLACEMENT_3D ( 'NONE', #340, #2037, #8030 ) ;
#2519 = ORIENTED_EDGE ( 'NONE', *, *, #10327, .T. ) ;
#2520 = DIRECTION ( 'NONE',  ( 0.000000000000000000, -0.8090169943749444537, -0.5877852522924771339 ) ) ;
#2521 = EDGE_CURVE ( 'NONE', #5672, #9010, #16367, .T. ) ;
#2522 = CARTESIAN_POINT ( 'NONE',  ( 1.761396867937162769, -5.421022142882388373, -10.00000000000000533 ) ) ;
#2523 = FACE_BOUND ( 'NONE', #8452, .T. ) ;
#2524 = VERTEX_POINT ( 'NONE', #8061 ) ;
#2525 = DIRECTION ( 'NONE',  ( 1.000000000000000000, 6.419766481290786633E-33, -0.000000000000000000 ) ) ;
#2526 = CARTESIAN_POINT ( 'NONE',  ( 12.86923836996420967, -11.47363181547641453, -32.00000000000000000 ) ) ;
#2527 = ORIENTED_EDGE ( 'NONE', *, *, #1214, .F. ) ;
#2528 = CARTESIAN_POINT ( 'NONE',  ( 0.000000000000000000, -24.34211360614305875, 7.909232158574721616 ) ) ;
#2529 =( NAMED_UNIT ( * ) PLANE_ANGLE_UNIT ( ) SI_UNIT ( $, .RADIAN. ) );
#2530 = CARTESIAN_POINT ( 'NONE',  ( -2.000000000000001776, 0.000000000000000000, 0.000000000000000000 ) ) ;
#2531 = ORIENTED_EDGE ( 'NONE', *, *, #12349, .F. ) ;
#2532 = LINE ( 'NONE', #7024, #3158 ) ;
#2533 = CARTESIAN_POINT ( 'NONE',  ( 9.000000000000005329, 0.5958122406255991210, 5.668774803599163192 ) ) ;
#2534 = FACE_OUTER_BOUND ( 'NONE', #18518, .T. ) ;
#2535 = EDGE_LOOP ( 'NONE', ( #11441, #1161, #5372, #16742 ) ) ;
#2536 = EDGE_CURVE ( 'NONE', #5021, #18417, #18673, .T. ) ;
#2537 = FACE_OUTER_BOUND ( 'NONE', #18242, .T. ) ;
#2538 = AXIS2_PLACEMENT_3D ( 'NONE', #3225, #4929, #10835 ) ;
#2539 = ORIENTED_EDGE ( 'NONE', *, *, #7560, .T. ) ;
#2540 = DIRECTION ( 'NONE',  ( 1.000000000000000000, 0.000000000000000000, 0.000000000000000000 ) ) ;
#2541 = DIRECTION ( 'NONE',  ( -1.000000000000000000, -0.000000000000000000, -0.000000000000000000 ) ) ;
#2542 = EDGE_LOOP ( 'NONE', ( #12122, #11121, #7342, #5440 ) ) ;
#2543 = DIRECTION ( 'NONE',  ( -1.000000000000000000, 0.000000000000000000, 0.000000000000000000 ) ) ;
#2544 = CARTESIAN_POINT ( 'NONE',  ( -2.444050593749990341, 4.233219804643887585, -6.468749997951615427 ) ) ;
#2545 = ADVANCED_FACE ( 'NONE', ( #7863 ), #577, .T. ) ;
#2546 = VERTEX_POINT ( 'NONE', #9384 ) ;
#2547 = EDGE_CURVE ( 'NONE', #9544, #8660, #7419, .T. ) ;
#2548 = ORIENTED_EDGE ( 'NONE', *, *, #15430, .F. ) ;
#2549 = DIRECTION ( 'NONE',  ( 0.000000000000000000, 0.000000000000000000, 1.000000000000000000 ) ) ;
#2550 = CIRCLE ( 'NONE', #12792, 0.9999999999999974465 ) ;
#2551 = DIRECTION ( 'NONE',  ( 0.000000000000000000, 0.5877852522924805756, -0.8090169943749421222 ) ) ;
#2552 = AXIS2_PLACEMENT_3D ( 'NONE', #15435, #15728, #18430 ) ;
#2553 = ORIENTED_EDGE ( 'NONE', *, *, #15596, .T. ) ;
#2554 = FACE_OUTER_BOUND ( 'NONE', #14176, .T. ) ;
#2555 = ORIENTED_EDGE ( 'NONE', *, *, #18715, .T. ) ;
#2556 = ADVANCED_FACE ( 'NONE', ( #14072 ), #15112, .T. ) ;
#2557 = EDGE_CURVE ( 'NONE', #18644, #562, #3563, .T. ) ;
#2558 = CYLINDRICAL_SURFACE ( 'NONE', #3258, 1.000000000000004441 ) ;
#2559 = CARTESIAN_POINT ( 'NONE',  ( 7.312499995903225525, -4.936344801571268093, -2.850000000000058265 ) ) ;
#2560 = ORIENTED_EDGE ( 'NONE', *, *, #11689, .F. ) ;
#2561 = CARTESIAN_POINT ( 'NONE',  ( 2.790000000000000036, 23.69843731927168662, 5.456805104201184697 ) ) ;
#2562 = CIRCLE ( 'NONE', #17287, 4.200000000000000178 ) ;
#2563 = AXIS2_PLACEMENT_3D ( 'NONE', #18503, #7690, #1505 ) ;
#2564 = DIRECTION ( 'NONE',  ( 0.000000000000000000, -1.224646799147353207E-16, 1.000000000000000000 ) ) ;
#2565 = FACE_OUTER_BOUND ( 'NONE', #14746, .T. ) ;
#2566 = FACE_OUTER_BOUND ( 'NONE', #18468, .T. ) ;
#2567 = CARTESIAN_POINT ( 'NONE',  ( 2.789999999999999147, 20.62201879784931435, -12.52067188844328882 ) ) ;
#2568 = CARTESIAN_POINT ( 'NONE',  ( 7.937500000000000000, 0.000000000000000000, 0.000000000000000000 ) ) ;
#2569 = VERTEX_POINT ( 'NONE', #11075 ) ;
#2570 = PRODUCT_RELATED_PRODUCT_CATEGORY ( 'part', '', ( #9709 ) ) ;
#2571 = CARTESIAN_POINT ( 'NONE',  ( 8.000000000000000000, 9.797174393178825657E-16, -33.00000000000000000 ) ) ;
#2572 = DIRECTION ( 'NONE',  ( -0.000000000000000000, 0.000000000000000000, 1.000000000000000000 ) ) ;
#2573 = UNCERTAINTY_MEASURE_WITH_UNIT (LENGTH_MEASURE( 1.000000000000000082E-05 ), #5287, 'distance_accuracy_value', 'NONE');
#2574 = CARTESIAN_POINT ( 'NONE',  ( -2.318398865532001363, 5.207209108562852684, -13.00000000000000533 ) ) ;
#2575 = CARTESIAN_POINT ( 'NONE',  ( 4.150607464521811174, 2.695436003842704764, -7.968749997951616315 ) ) ;
#2576 = AXIS2_PLACEMENT_3D ( 'NONE', #10946, #14446, #8238 ) ;
#2577 = CARTESIAN_POINT ( 'NONE',  ( 0.9027913098498566713, 5.699999999999999289, -12.81249999590322552 ) ) ;
#2578 = ORIENTED_EDGE ( 'NONE', *, *, #18821, .F. ) ;
#2579 = EDGE_CURVE ( 'NONE', #9276, #2546, #4554, .T. ) ;
#2580 = CYLINDRICAL_SURFACE ( 'NONE', #14443, 13.19999999999999929 ) ;
#2581 = EDGE_CURVE ( 'NONE', #18102, #10126, #4676, .T. ) ;
#2582 = CARTESIAN_POINT ( 'NONE',  ( 5.700000000000001954, 0.2987243419133224775, -10.47794484381774538 ) ) ;
#2583 = ORIENTED_EDGE ( 'NONE', *, *, #11378, .T. ) ;
#2584 = CARTESIAN_POINT ( 'NONE',  ( 7.968749997951616315, -2.695436003842674566, -4.150607464521828938 ) ) ;
#2585 = CARTESIAN_POINT ( 'NONE',  ( 0.7592463977762118343, 4.828194074574732930, -27.14986936243569460 ) ) ;
#2586 = CARTESIAN_POINT ( 'NONE',  ( 2.765633920072238183, -18.55949924794904504, 16.37294372382852004 ) ) ;
#2587 = DIRECTION ( 'NONE',  ( 1.000000000000000000, 0.000000000000000000, 0.000000000000000000 ) ) ;
#2588 = SHAPE_REPRESENTATION ( 'machine screw nut hex_ai_MSHXNUT 0.375-16-S-N', ( #16724 ), #5229 ) ;
#2589 = ADVANCED_FACE ( 'NONE', ( #9281 ), #1689, .T. ) ;
#2590 = ORIENTED_EDGE ( 'NONE', *, *, #16110, .T. ) ;
#2591 = AXIS2_PLACEMENT_3D ( 'NONE', #12649, #18642, #11146 ) ;
#2592 = AXIS2_PLACEMENT_3D ( 'NONE', #19419, #5705, #19622 ) ;
#2593 = DIRECTION ( 'NONE',  ( 0.000000000000000000, 0.000000000000000000, 1.000000000000000000 ) ) ;
#2594 = DIRECTION ( 'NONE',  ( 1.000000000000000000, -0.000000000000000000, -0.000000000000000000 ) ) ;
#2595 = CIRCLE ( 'NONE', #8359, 1.000000000000003109 ) ;
#2596 = CARTESIAN_POINT ( 'NONE',  ( 0.000000000000000000, -18.28042085475288303, 15.74360496233377305 ) ) ;
#2597 = VERTEX_POINT ( 'NONE', #12384 ) ;
#2598 = EDGE_CURVE ( 'NONE', #19366, #19037, #7085, .T. ) ;
#2599 = CARTESIAN_POINT ( 'NONE',  ( 0.1855657168891856057, 12.84444904262024956, 22.53097606932990260 ) ) ;
#2600 = VERTEX_POINT ( 'NONE', #6947 ) ;
#2601 = ADVANCED_FACE ( 'NONE', ( #8659 ), #19260, .T. ) ;
#2602 = CARTESIAN_POINT ( 'NONE',  ( 1.734723475976807094E-15, 9.165435523385314198, -0.7089489049740167470 ) ) ;
#2603 = CARTESIAN_POINT ( 'NONE',  ( -1.761396867937200739, 5.421022142882375938, -11.31249999590322375 ) ) ;
#2604 = CARTESIAN_POINT ( 'NONE',  ( 2.765633920072236851, 24.15498966839963302, 5.391175441198700291 ) ) ;
#2605 = CYLINDRICAL_SURFACE ( 'NONE', #8560, 1.000000000000002665 ) ;
#2606 = ORIENTED_EDGE ( 'NONE', *, *, #12764, .T. ) ;
#2607 = CARTESIAN_POINT ( 'NONE',  ( 2.999999999999998224, 0.000000000000000000, 0.000000000000000000 ) ) ;
#2608 = CARTESIAN_POINT ( 'NONE',  ( 1.749999999999998002, 0.000000000000000000, 0.000000000000000000 ) ) ;
#2609 = CIRCLE ( 'NONE', #13160, 8.265000000000021885 ) ;
#2610 = ORIENTED_EDGE ( 'NONE', *, *, #7522, .T. ) ;
#2611 = VECTOR ( 'NONE', #17682, 1000.000000000000000 ) ;
#2612 = AXIS2_PLACEMENT_3D ( 'NONE', #15614, #1804, #12217 ) ;
#2613 = DIRECTION ( 'NONE',  ( 1.000000000000000000, 0.000000000000000000, 0.000000000000000000 ) ) ;
#2614 = CARTESIAN_POINT ( 'NONE',  ( 2.789999999999999147, 0.000000000000000000, 0.000000000000000000 ) ) ;
#2615 = ORIENTED_EDGE ( 'NONE', *, *, #18615, .T. ) ;
#2616 = CARTESIAN_POINT ( 'NONE',  ( 1.280903732194454303, 4.780397808154257078, -8.968749997951611874 ) ) ;
#2617 = CARTESIAN_POINT ( 'NONE',  ( 0.000000000000000000, 0.000000000000000000, -33.00000000000000000 ) ) ;
#2618 = CARTESIAN_POINT ( 'NONE',  ( 0.0003207540509381473352, -20.70663861606275447, -12.51925356660783528 ) ) ;
#2619 = ORIENTED_EDGE ( 'NONE', *, *, #10872, .T. ) ;
#2620 = DIRECTION ( 'NONE',  ( 0.000000000000000000, 0.000000000000000000, 1.000000000000000000 ) ) ;
#2621 = EDGE_LOOP ( 'NONE', ( #968, #5215, #13361, #10275 ) ) ;
#2622 = CARTESIAN_POINT ( 'NONE',  ( -20.63749999999999929, 0.000000000000000000, 0.000000000000000000 ) ) ;
#2623 = CIRCLE ( 'NONE', #8377, 2.524999999999995914 ) ;
#2624 = EDGE_LOOP ( 'NONE', ( #11380, #14427, #9352, #15291 ) ) ;
#2625 = AXIS2_PLACEMENT_3D ( 'NONE', #8074, #17387, #3675 ) ;
#2626 = CARTESIAN_POINT ( 'NONE',  ( 1.799999999999999600, 0.000000000000000000, -8.000000000000000000 ) ) ;
#2627 = CARTESIAN_POINT ( 'NONE',  ( 2.999999999999998224, 3.950217066951266176, 3.681818181818181213 ) ) ;
#2628 = DIRECTION ( 'NONE',  ( -1.000000000000000000, -6.419766481290788001E-33, -0.000000000000000000 ) ) ;
#2629 = DIRECTION ( 'NONE',  ( 0.000000000000000000, -1.000000000000000000, 0.000000000000000000 ) ) ;
#2630 = CARTESIAN_POINT ( 'NONE',  ( 17.96448111170888851, 1.130229351527639148, -32.00000000000000000 ) ) ;
#2631 = CARTESIAN_POINT ( 'NONE',  ( 2.999999999999998224, -3.950217066951263956, -3.681818181818183877 ) ) ;
#2632 = ORIENTED_EDGE ( 'NONE', *, *, #10042, .T. ) ;
#2633 = AXIS2_PLACEMENT_3D ( 'NONE', #12364, #9262, #12262 ) ;
#2634 = MANIFOLD_SOLID_BREP ( 'Cut-Extrude-Thin1', #18032 ) ;
#2635 = DIRECTION ( 'NONE',  ( -0.000000000000000000, -0.000000000000000000, 1.000000000000000000 ) ) ;
#2636 = CIRCLE ( 'NONE', #14472, 1.199999999999999734 ) ;
#2637 = ORIENTED_EDGE ( 'NONE', *, *, #3917, .F. ) ;
#2638 = DIRECTION ( 'NONE',  ( 0.000000000000000000, 0.000000000000000000, 1.000000000000000000 ) ) ;
#2639 = B_SPLINE_CURVE_WITH_KNOTS ( 'NONE', 3,
 ( #18612, #18707, #10917, #18810, #5199, #11317 ),
 .UNSPECIFIED., .F., .F.,
 ( 4, 2, 4 ),
 ( 4.462636882206429356E-07, 0.001879885203074806513, 0.003759324142461392161 ),
 .UNSPECIFIED. ) ;
#2640 = CARTESIAN_POINT ( 'NONE',  ( 2.789999999999999147, 0.000000000000000000, 0.000000000000000000 ) ) ;
#2641 = VECTOR ( 'NONE', #12255, 1000.000000000000000 ) ;
#2642 = DIRECTION ( 'NONE',  ( -0.000000000000000000, -0.000000000000000000, 1.000000000000000000 ) ) ;
#2643 = VECTOR ( 'NONE', #18602, 1000.000000000000000 ) ;
#2644 = LINE ( 'NONE', #18357, #18320 ) ;
#2645 = VERTEX_POINT ( 'NONE', #8564 ) ;
#2646 = CARTESIAN_POINT ( 'NONE',  ( 0.000000000000000000, 0.000000000000000000, 0.000000000000000000 ) ) ;
#2647 = LINE ( 'NONE', #12066, #11270 ) ;
#2648 = EDGE_CURVE ( 'NONE', #6118, #12561, #17683, .T. ) ;
#2649 = ORIENTED_EDGE ( 'NONE', *, *, #14169, .F. ) ;
#2650 = ORIENTED_EDGE ( 'NONE', *, *, #14058, .F. ) ;
#2651 = CYLINDRICAL_SURFACE ( 'NONE', #11136, 1.000000000000002665 ) ;
#2652 = APPLICATION_CONTEXT ( 'automotive_design' ) ;
#2653 = DIRECTION ( 'NONE',  ( -1.000000000000000000, 0.000000000000000000, -0.000000000000000000 ) ) ;
#2654 = ORIENTED_EDGE ( 'NONE', *, *, #1104, .F. ) ;
#2655 = DIRECTION ( 'NONE',  ( 0.000000000000000000, 0.000000000000000000, 1.000000000000000000 ) ) ;
#2656 = ORIENTED_EDGE ( 'NONE', *, *, #954, .F. ) ;
#2657 = CARTESIAN_POINT ( 'NONE',  ( -15.19790265903627180, 9.644882309621941374, -32.00000000000000000 ) ) ;
#2658 = VECTOR ( 'NONE', #17100, 1000.000000000000114 ) ;
#2659 = CARTESIAN_POINT ( 'NONE',  ( 0.006930995026450116094, -5.408431875071277872, -23.92277630352801054 ) ) ;
#2660 = VERTEX_POINT ( 'NONE', #18973 ) ;
#2661 = CARTESIAN_POINT ( 'NONE',  ( -39.64101615137792578, 82.80384757729314060, 37.99999999999999289 ) ) ;
#2662 = EDGE_CURVE ( 'NONE', #4037, #9386, #15880, .T. ) ;
#2663 = DIRECTION ( 'NONE',  ( 0.000000000000000000, 0.000000000000000000, -1.000000000000000000 ) ) ;
#2664 = CARTESIAN_POINT ( 'NONE',  ( -5.312660008432906977, 6.098169837403609961, -0.06756670027994018946 ) ) ;
#2665 = CARTESIAN_POINT ( 'NONE',  ( 1.800000000000000044, 0.000000000000000000, 0.000000000000000000 ) ) ;
#2666 = PRODUCT ( 'plain washer clevis pin grade a_iso_ISO 8738 - 12', 'plain washer clevis pin grade a_iso_ISO 8738 - 12', '', ( #6332 ) ) ;
#2667 = CARTESIAN_POINT ( 'NONE',  ( 13.86923836996420789, -11.47363181547641453, 32.00000000000000000 ) ) ;
#2668 = DIRECTION ( 'NONE',  ( -0.000000000000000000, -0.000000000000000000, 1.000000000000000000 ) ) ;
#2669 = EDGE_CURVE ( 'NONE', #2248, #6546, #11911, .T. ) ;
#2670 = AXIS2_PLACEMENT_3D ( 'NONE', #5715, #2425, #11931 ) ;
#2671 = ORIENTED_EDGE ( 'NONE', *, *, #18158, .F. ) ;
#2672 = LINE ( 'NONE', #8788, #16879 ) ;
#2673 = DIRECTION ( 'NONE',  ( -1.000000000000000000, -0.000000000000000000, -0.000000000000000000 ) ) ;
#2674 = CARTESIAN_POINT ( 'NONE',  ( -5.387740456496205255, 2.068159791354258648, -10.50000000000000533 ) ) ;
#2675 = CARTESIAN_POINT ( 'NONE',  ( 2.789999999999999147, 20.70663861606293210, -15.04425356660737556 ) ) ;
#2676 = CIRCLE ( 'NONE', #16434, 22.00000000000000355 ) ;
#2677 = DIRECTION ( 'NONE',  ( 0.000000000000000000, 0.000000000000000000, -1.000000000000000000 ) ) ;
#2678 = VERTEX_POINT ( 'NONE', #7038 ) ;
#2679 = CARTESIAN_POINT ( 'NONE',  ( 0.000000000000000000, 0.000000000000000000, 0.000000000000000000 ) ) ;
#2680 = CARTESIAN_POINT ( 'NONE',  ( 5.668774803599163192, 0.5958122406255991210, -10.31249999590322552 ) ) ;
#2681 = EDGE_LOOP ( 'NONE', ( #14546, #4895, #5342, #15515 ) ) ;
#2682 = CARTESIAN_POINT ( 'NONE',  ( 9.968749997951617203, 0.2590123213421660631, -4.942249507334553371 ) ) ;
#2683 = CONICAL_SURFACE ( 'NONE', #16139, 6.735000000000022524, 0.3653297453805129935 ) ;
#2684 = EDGE_CURVE ( 'NONE', #12845, #19252, #3862, .T. ) ;
#2685 = CARTESIAN_POINT ( 'NONE',  ( 8.312499995903225525, -5.575441324182703440, 1.185096637661176677 ) ) ;
#2686 = CARTESIAN_POINT ( 'NONE',  ( 13.00000000000000178, 0.000000000000000000, 6.500000000000002665 ) ) ;
#2687 = FACE_OUTER_BOUND ( 'NONE', #2789, .T. ) ;
#2688 = EDGE_CURVE ( 'NONE', #16413, #17466, #13505, .T. ) ;
#2689 = ORIENTED_EDGE ( 'NONE', *, *, #4751, .F. ) ;
#2690 = AXIS2_PLACEMENT_3D ( 'NONE', #13346, #5544, #3953 ) ;
#2691 = CARTESIAN_POINT ( 'NONE',  ( 0.000000000000000000, -9.324097380959594616, 22.25075486061734509 ) ) ;
#2692 = CARTESIAN_POINT ( 'NONE',  ( 3.846120219227923798, -3.114526743279282250, -12.34374999795161543 ) ) ;
#2693 = SURFACE_STYLE_USAGE ( .BOTH. , #10220 ) ;
#2694 = ORIENTED_EDGE ( 'NONE', *, *, #12053, .T. ) ;
#2695 = ADVANCED_FACE ( 'NONE', ( #959 ), #16118, .T. ) ;
#2696 = CARTESIAN_POINT ( 'NONE',  ( 0.5279273620711159021, 12.96450951081217084, 23.73240184472501113 ) ) ;
#2697 = ORIENTED_EDGE ( 'NONE', *, *, #7222, .F. ) ;
#2698 = CYLINDRICAL_SURFACE ( 'NONE', #18844, 1.000000000000002665 ) ;
#2699 = CIRCLE ( 'NONE', #16683, 28.06981291497571007 ) ;
#2700 = CARTESIAN_POINT ( 'NONE',  ( 9.968749997951617203, 4.409619785863906571, -2.246813503491833508 ) ) ;
#2701 = DIRECTION ( 'NONE',  ( 0.000000000000000000, 0.000000000000000000, -1.000000000000000000 ) ) ;
#2702 = CARTESIAN_POINT ( 'NONE',  ( 4.465502636338025688, -1.988169868018592412, -14.84374999795161543 ) ) ;
#2703 = ORIENTED_EDGE ( 'NONE', *, *, #713, .T. ) ;
#2704 = CARTESIAN_POINT ( 'NONE',  ( 1.749999999999998002, 19.67366047555530528, 20.02152543075352753 ) ) ;
#2705 = EDGE_CURVE ( 'NONE', #9559, #13272, #16076, .T. ) ;
#2706 = DIRECTION ( 'NONE',  ( -1.000000000000000000, 0.000000000000000000, 0.000000000000000000 ) ) ;
#2707 = AXIS2_PLACEMENT_3D ( 'NONE', #7173, #4100, #13493 ) ;
#2708 = ORIENTED_EDGE ( 'NONE', *, *, #16548, .T. ) ;
#2709 =( BOUNDED_CURVE ( )  B_SPLINE_CURVE ( 2, ( #9967, #15865, #18957, #11646, #16253, #19245, #8551, #6837, #14465, #17561, #11365, #762, #14660 ),
 .UNSPECIFIED., .F., .F. ) 
 B_SPLINE_CURVE_WITH_KNOTS ( ( 3, 2, 2, 2, 2, 2, 3 ),
 ( 0.000000000000000000, 0.05000000000000000278, 0.1000000000000000056, 0.1499999999999999944, 0.2000000000000000111, 0.2500000000000000000, 0.2843253191101272614 ),
 .UNSPECIFIED. ) 
 CURVE ( )  GEOMETRIC_REPRESENTATION_ITEM ( )  RATIONAL_B_SPLINE_CURVE ( ( 1.000000000000000000, 0.9876883405951377704, 1.000000000000000000, 0.9876883405951377704, 1.000000000000000000, 0.9876883405951377704, 1.000000000000000000, 0.9876883405951377704, 1.000000000000000000, 0.9876883405951377704, 1.000000000000000000, 0.9915479672430580482, 0.9947006833465674713 ) ) 
 REPRESENTATION_ITEM ( '' )  );
#2710 = EDGE_CURVE ( 'NONE', #1471, #10072, #2647, .T. ) ;
#2711 = ADVANCED_FACE ( 'NONE', ( #7138 ), #14866, .F. ) ;
#2712 = CARTESIAN_POINT ( 'NONE',  ( 5.510910596163084625E-16, 18.00000000000000355, 32.00000000000000000 ) ) ;
#2713 = CARTESIAN_POINT ( 'NONE',  ( -3.383411828340740850E-14, -4.888101187500000222, -11.84374999795161365 ) ) ;
#2714 = ORIENTED_EDGE ( 'NONE', *, *, #12629, .F. ) ;
#2715 = CARTESIAN_POINT ( 'NONE',  ( 0.5109457054261784537, 4.861323657744407001, -8.843749997951615427 ) ) ;
#2716 = FACE_OUTER_BOUND ( 'NONE', #11184, .T. ) ;
#2717 = CARTESIAN_POINT ( 'NONE',  ( 11.84374999795161365, -2.444050593750019651, 4.233219804643871598 ) ) ;
#2718 = ORIENTED_EDGE ( 'NONE', *, *, #18316, .F. ) ;
#2719 = DIRECTION ( 'NONE',  ( 0.000000000000000000, 0.000000000000000000, -1.000000000000000000 ) ) ;
#2720 = ORIENTED_EDGE ( 'NONE', *, *, #12633, .T. ) ;
#2721 = DIRECTION ( 'NONE',  ( 1.000000000000000000, 0.000000000000000000, 0.000000000000000000 ) ) ;
#2722 = CIRCLE ( 'NONE', #5285, 3.797000000000000597 ) ;
#2723 = VERTEX_POINT ( 'NONE', #2947 ) ;
#2724 = CARTESIAN_POINT ( 'NONE',  ( 0.7592463834391182109, 24.80264696524898937, -12.05220173035413112 ) ) ;
#2725 = CIRCLE ( 'NONE', #14572, 8.000000000000000000 ) ;
#2726 = CARTESIAN_POINT ( 'NONE',  ( 7.671566133830872047, 15.77352024078954784, 32.00000000000000000 ) ) ;
#2727 = CARTESIAN_POINT ( 'NONE',  ( -11.58013454126452579, -14.56230589874905235, -32.00000000000000000 ) ) ;
#2728 = CARTESIAN_POINT ( 'NONE',  ( 7.500000000000005329, -5.763142191869158992, 0.3020334839682081163 ) ) ;
#2729 = DIRECTION ( 'NONE',  ( 0.000000000000000000, 0.7315216790650492795, 0.6818181818181815457 ) ) ;
#2730 = VERTEX_POINT ( 'NONE', #8864 ) ;
#2731 = EDGE_CURVE ( 'NONE', #2257, #15969, #5945, .T. ) ;
#2732 = CARTESIAN_POINT ( 'NONE',  ( 8.671566133830875600, 15.77352024078954784, -35.00000000000000000 ) ) ;
#2733 = DIRECTION ( 'NONE',  ( 0.000000000000000000, 0.000000000000000000, -1.000000000000000000 ) ) ;
#2734 = EDGE_CURVE ( 'NONE', #18318, #12686, #18638, .T. ) ;
#2735 = AXIS2_PLACEMENT_3D ( 'NONE', #3430, #6406, #1924 ) ;
#2736 = VERTEX_POINT ( 'NONE', #10664 ) ;
#2737 = CIRCLE ( 'NONE', #5306, 3.000000000000000000 ) ;
#2738 = DIRECTION ( 'NONE',  ( 1.000000000000000000, 0.000000000000000000, 0.000000000000000000 ) ) ;
#2739 = CARTESIAN_POINT ( 'NONE',  ( -30.00000000000000000, 8.000000000000000000, 0.000000000000000000 ) ) ;
#2740 = CARTESIAN_POINT ( 'NONE',  ( 4.942249507334556036, -0.2590123213421313686, -9.968749997951617203 ) ) ;
#2741 = FACE_OUTER_BOUND ( 'NONE', #14563, .T. ) ;
#2742 = ORIENTED_EDGE ( 'NONE', *, *, #14377, .F. ) ;
#2743 = CARTESIAN_POINT ( 'NONE',  ( 17.28688694438834972, -7.664027248171309203, -32.00000000000000000 ) ) ;
#2744 = B_SPLINE_CURVE_WITH_KNOTS ( 'NONE', 3,
 ( #13830, #9029, #6305, #3119, #2816, #4516 ),
 .UNSPECIFIED., .F., .F.,
 ( 4, 2, 4 ),
 ( 2.586195665686417350E-07, 0.001878649493629684251, 0.003757040367692799938 ),
 .UNSPECIFIED. ) ;
#2745 = DIRECTION ( 'NONE',  ( 0.000000000000000000, 0.000000000000000000, 1.000000000000000000 ) ) ;
#2746 = CARTESIAN_POINT ( 'NONE',  ( 1.493657965219523875, 5.574407415329156734, -8.500000000000007105 ) ) ;
#2747 = EDGE_LOOP ( 'NONE', ( #11610, #3472 ) ) ;
#2748 = ORIENTED_EDGE ( 'NONE', *, *, #3055, .T. ) ;
#2749 = CARTESIAN_POINT ( 'NONE',  ( 17.68117051311639898, -3.372863662543048591, 32.00000000000000000 ) ) ;
#2750 = AXIS2_PLACEMENT_3D ( 'NONE', #17427, #1002, #14528 ) ;
#2751 = CARTESIAN_POINT ( 'NONE',  ( 7.968749997951616315, 2.695436003842704764, 4.150607464521812062 ) ) ;
#2752 = VECTOR ( 'NONE', #14520, 1000.000000000000000 ) ;
#2753 = ORIENTED_EDGE ( 'NONE', *, *, #8979, .F. ) ;
#2754 = ADVANCED_FACE ( 'NONE', ( #16773 ), #12549, .T. ) ;
#2755 = FACE_OUTER_BOUND ( 'NONE', #18781, .T. ) ;
#2756 = ORIENTED_EDGE ( 'NONE', *, *, #12082, .T. ) ;
#2757 = DIRECTION ( 'NONE',  ( -1.000000000000000000, -0.000000000000000000, -0.000000000000000000 ) ) ;
#2758 = CARTESIAN_POINT ( 'NONE',  ( 1.999999999999999556, -5.000000000000001776, 37.99999999999999289 ) ) ;
#2759 = EDGE_LOOP ( 'NONE', ( #5210, #19294, #7443, #4978 ) ) ;
#2760 = DIRECTION ( 'NONE',  ( -0.000000000000000000, -0.000000000000000000, 1.000000000000000000 ) ) ;
#2761 = EDGE_CURVE ( 'NONE', #1129, #15138, #17026, .T. ) ;
#2762 = TOROIDAL_SURFACE ( 'NONE', #13627, 8.800000000000022027, 0.1999999999999994282 ) ;
#2763 = AXIS2_PLACEMENT_3D ( 'NONE', #10589, #7963, #18482 ) ;
#2764 = CARTESIAN_POINT ( 'NONE',  ( 13.84374999795161543, 3.954556930911862000, 2.873153789725825025 ) ) ;
#2765 = CARTESIAN_POINT ( 'NONE',  ( 5.142044285764733935, -2.620002426024580000, -8.812499995903225525 ) ) ;
#2766 = VERTEX_POINT ( 'NONE', #10760 ) ;
#2767 = EDGE_CURVE ( 'NONE', #2736, #5005, #1456, .T. ) ;
#2768 = DIRECTION ( 'NONE',  ( 1.000000000000000000, 0.000000000000000000, 0.000000000000000000 ) ) ;
#2769 = CARTESIAN_POINT ( 'NONE',  ( 0.02436607992776411782, -16.37294372382844543, -18.55949924794910544 ) ) ;
#2770 = VERTEX_POINT ( 'NONE', #15658 ) ;
#2771 = CARTESIAN_POINT ( 'NONE',  ( -15.28688694438835505, -7.664027248171298545, 35.00000000000000000 ) ) ;
#2772 = DIRECTION ( 'NONE',  ( -1.000000000000000000, 0.000000000000000000, 0.000000000000000000 ) ) ;
#2773 = PRODUCT_DEFINITION_CONTEXT ( 'detailed design', #9450, 'design' ) ;
#2774 = LINE ( 'NONE', #8890, #334 ) ;
#2775 = CARTESIAN_POINT ( 'NONE',  ( 2.444050593750020095, 4.233219804643871598, -6.468749997951615427 ) ) ;
#2776 = AXIS2_PLACEMENT_3D ( 'NONE', #16984, #3266, #15183 ) ;
#2777 = CYLINDRICAL_SURFACE ( 'NONE', #6956, 14.00000000000000178 ) ;
#2778 = AXIS2_PLACEMENT_3D ( 'NONE', #14754, #13058, #2729 ) ;
#2779 = VERTEX_POINT ( 'NONE', #4953 ) ;
#2780 = DIRECTION ( 'NONE',  ( 0.000000000000000000, 0.000000000000000000, 1.000000000000000000 ) ) ;
#2781 = CARTESIAN_POINT ( 'NONE',  ( -4.150607464521828938, -2.695436003842674122, -7.968749997951616315 ) ) ;
#2782 = B_SPLINE_CURVE_WITH_KNOTS ( 'NONE', 3,
 ( #10099, #11397, #13092, #6775 ),
 .UNSPECIFIED., .F., .F.,
 ( 4, 4 ),
 ( 2.034713381942717888E-07, 0.0006045424356927869836 ),
 .UNSPECIFIED. ) ;
#2783 = VERTEX_POINT ( 'NONE', #6428 ) ;
#2784 = CARTESIAN_POINT ( 'NONE',  ( 8.843749997951615427, 1.988169868018562436, 4.465502636338039011 ) ) ;
#2785 = EDGE_CURVE ( 'NONE', #8438, #17152, #19249, .T. ) ;
#2786 = CARTESIAN_POINT ( 'NONE',  ( 6.656249997951614539, 4.936344801571289409, 2.850000000000024070 ) ) ;
#2787 = CARTESIAN_POINT ( 'NONE',  ( 13.00000000000000000, 4.125339889944109828, -2.622041954598519187 ) ) ;
#2788 = CARTESIAN_POINT ( 'NONE',  ( 2.789999999999999147, -24.63872515616080960, -2.336989772644527008 ) ) ;
#2789 = EDGE_LOOP ( 'NONE', ( #15950, #5872, #15281, #4846, #8667, #14112, #484, #5555 ) ) ;
#2790 = CIRCLE ( 'NONE', #13987, 1.000000000000002665 ) ;
#2791 = CARTESIAN_POINT ( 'NONE',  ( 0.000000000000000000, 0.000000000000000000, -3.323500000000020993 ) ) ;
#2792 = DIRECTION ( 'NONE',  ( -9.559896011775280412E-17, -0.7806247497997995666, -0.6250000000000002220 ) ) ;
#2793 = CIRCLE ( 'NONE', #13352, 2.524999999999996803 ) ;
#2794 = CARTESIAN_POINT ( 'NONE',  ( 14.46874999795161720, -2.873153789725797935, -3.954556930911881096 ) ) ;
#2795 = ORIENTED_EDGE ( 'NONE', *, *, #5804, .F. ) ;
#2796 = DIRECTION ( 'NONE',  ( 1.000000000000000000, 0.000000000000000000, 0.000000000000000000 ) ) ;
#2797 = ORIENTED_EDGE ( 'NONE', *, *, #12498, .T. ) ;
#2798 = DIRECTION ( 'NONE',  ( 0.000000000000000000, 0.000000000000000000, 1.000000000000000000 ) ) ;
#2799 = DIRECTION ( 'NONE',  ( 0.000000000000000000, 5.329070518200751394E-15, 1.000000000000000000 ) ) ;
#2800 = AXIS2_PLACEMENT_3D ( 'NONE', #8005, #1814, #2012 ) ;
#2801 = ADVANCED_FACE ( 'NONE', ( #18363 ), #16964, .F. ) ;
#2802 = ADVANCED_FACE ( 'NONE', ( #3351 ), #8707, .T. ) ;
#2803 = CARTESIAN_POINT ( 'NONE',  ( 12.99999999999998046, -4.467995623377355230, -2.612285395956023493 ) ) ;
#2804 = CARTESIAN_POINT ( 'NONE',  ( 0.5109457054261780096, 4.861323657744407001, -8.843749997951615427 ) ) ;
#2805 = ORIENTED_EDGE ( 'NONE', *, *, #13441, .F. ) ;
#2806 = CARTESIAN_POINT ( 'NONE',  ( -3.270778111535363131, -3.632567103900500971, -10.46874999795161720 ) ) ;
#2807 = CARTESIAN_POINT ( 'NONE',  ( -1.310841663519413114, 0.000000000000000000, 4.000000000000000000 ) ) ;
#2808 = AXIS2_PLACEMENT_3D ( 'NONE', #6377, #13806, #1706 ) ;
#2809 = ORIENTED_EDGE ( 'NONE', *, *, #15833, .F. ) ;
#2810 = VECTOR ( 'NONE', #5879, 1000.000000000000000 ) ;
#2811 = CARTESIAN_POINT ( 'NONE',  ( -4.409619785863906571, 2.246813503491833508, -7.968749997951616315 ) ) ;
#2812 = CARTESIAN_POINT ( 'NONE',  ( 2.765633920072235075, 24.63872515616082737, -2.336989772644355590 ) ) ;
#2813 = EDGE_LOOP ( 'NONE', ( #17249, #3967, #4971, #10523, #8736, #9617, #19605 ) ) ;
#2814 = CARTESIAN_POINT ( 'NONE',  ( 0.000000000000000000, -24.04302995059967429, 1.991882183130232242 ) ) ;
#2815 = CARTESIAN_POINT ( 'NONE',  ( 1.799999999999999600, 0.000000000000000000, 0.000000000000000000 ) ) ;
#2816 = CARTESIAN_POINT ( 'NONE',  ( 0.7589665089996495695, 24.80232951178378187, 12.05173163741731202 ) ) ;
#2817 = EDGE_LOOP ( 'NONE', ( #12909, #6116, #11935, #9643 ) ) ;
#2818 = CARTESIAN_POINT ( 'NONE',  ( -10.00000000000000000, 0.000000000000000000, 0.000000000000000000 ) ) ;
#2819 = EDGE_LOOP ( 'NONE', ( #14388, #2416 ) ) ;
#2821 = CARTESIAN_POINT ( 'NONE',  ( 6.468749997951615427, 4.233219804643871598, 2.444050593750020095 ) ) ;
#2820 = AXIS2_PLACEMENT_3D ( 'NONE', #5950, #18174, #8662 ) ;
#2822 = EDGE_LOOP ( 'NONE', ( #1772, #15376, #17903, #478 ) ) ;
#2823 = CARTESIAN_POINT ( 'NONE',  ( 6.656249997951614539, -3.980288726281172656E-14, 5.700000000000001066 ) ) ;
#2824 = DIRECTION ( 'NONE',  ( 0.000000000000000000, 0.000000000000000000, -1.000000000000000000 ) ) ;
#2825 = DIRECTION ( 'NONE',  ( -1.000000000000000000, 0.000000000000000000, 0.000000000000000000 ) ) ;
#2826 = DIRECTION ( 'NONE',  ( 1.000000000000000000, 0.000000000000000000, 0.000000000000000000 ) ) ;
#2827 = CARTESIAN_POINT ( 'NONE',  ( 12.99999999999999112, 4.467995623377368553, 2.612285395955995515 ) ) ;
#2828 = ORIENTED_EDGE ( 'NONE', *, *, #3804, .T. ) ;
#2829 = B_SPLINE_CURVE_WITH_KNOTS ( 'NONE', 3,
 ( #18586, #8179, #18683, #4785 ),
 .UNSPECIFIED., .F., .F.,
 ( 4, 4 ),
 ( 0.005258105385878676132, 0.005948373736081387537 ),
 .UNSPECIFIED. ) ;
#2830 = CARTESIAN_POINT ( 'NONE',  ( -3.954556930911881096, -2.873153789725797935, -14.84374999795161543 ) ) ;
#2831 =( BOUNDED_CURVE ( )  B_SPLINE_CURVE ( 2, ( #15093, #1389, #4092, #2674, #7468, #7362, #16297, #4287, #2574, #7166, #19386 ),
 .UNSPECIFIED., .F., .F. ) 
 B_SPLINE_CURVE_WITH_KNOTS ( ( 3, 2, 2, 2, 2, 3 ),
 ( 0.1666819079834106210, 0.2000000000000000111, 0.2500000000000000000, 0.2999999999999999889, 0.3499999999999999778, 0.4000000000000000222 ),
 .UNSPECIFIED. ) 
 CURVE ( )  GEOMETRIC_REPRESENTATION_ITEM ( )  RATIONAL_B_SPLINE_CURVE ( ( 0.9945256517182514688, 0.9917959799814378696, 1.000000000000000000, 0.9876883405951377704, 1.000000000000000000, 0.9876883405951377704, 1.000000000000000000, 0.9876883405951377704, 1.000000000000000000, 0.9876883405951377704, 1.000000000000000000 ) ) 
 REPRESENTATION_ITEM ( '' )  );
#2832 =( REPRESENTATION_RELATIONSHIP ('NONE','NONE', #18211, #4652 ) REPRESENTATION_RELATIONSHIP_WITH_TRANSFORMATION ( #2242 )SHAPE_REPRESENTATION_RELATIONSHIP( ) );
#2833 = CARTESIAN_POINT ( 'NONE',  ( 0.7589665349472735079, 4.828387785248019703, 27.14933624560909919 ) ) ;
#2834 = EDGE_CURVE ( 'NONE', #2110, #17016, #10627, .T. ) ;
#2835 = EDGE_CURVE ( 'NONE', #9369, #19326, #15464, .T. ) ;
#2836 = AXIS2_PLACEMENT_3D ( 'NONE', #19340, #16345, #11745 ) ;
#2837 = EDGE_LOOP ( 'NONE', ( #2104, #1950 ) ) ;
#2838 = DIRECTION ( 'NONE',  ( 0.000000000000000000, 0.000000000000000000, -1.000000000000000000 ) ) ;
#2839 = DIRECTION ( 'NONE',  ( -1.000000000000000000, -1.224646799147353207E-16, -0.000000000000000000 ) ) ;
#2840 = ORIENTED_EDGE ( 'NONE', *, *, #9859, .F. ) ;
#2841 = DIRECTION ( 'NONE',  ( 0.000000000000000000, 0.000000000000000000, 1.000000000000000000 ) ) ;
#2842 = CARTESIAN_POINT ( 'NONE',  ( 3.143139765844590983, -4.840010801796506890, -12.50000000000000533 ) ) ;
#2843 = DIRECTION ( 'NONE',  ( -1.000000000000000000, -0.000000000000000000, -0.000000000000000000 ) ) ;
#2844 = ORIENTED_EDGE ( 'NONE', *, *, #9903, .F. ) ;
#2845 = CARTESIAN_POINT ( 'NONE',  ( 17.11901729331276556, 5.562305898749055011, 32.00000000000000000 ) ) ;
#2846 = EDGE_LOOP ( 'NONE', ( #4452, #8328 ) ) ;
#2847 = DIRECTION ( 'NONE',  ( -1.063860785392510441E-16, -1.878311291571669384E-17, 1.000000000000000000 ) ) ;
#2848 = CARTESIAN_POINT ( 'NONE',  ( 1.185096637661176677, -5.575441324182703440, -7.000000000000005329 ) ) ;
#2849 = ORIENTED_EDGE ( 'NONE', *, *, #10988, .T. ) ;
#2850 = VERTEX_POINT ( 'NONE', #13760 ) ;
#2851 = LINE ( 'NONE', #13565, #19746 ) ;
#2852 = TOROIDAL_SURFACE ( 'NONE', #2213, 6.200000000000020606, 0.2000000000000005107 ) ;
#2853 = CARTESIAN_POINT ( 'NONE',  ( 3.814044456245502701, 4.235925505221138643, -11.31249999590322375 ) ) ;
#2854 = EDGE_CURVE ( 'NONE', #10624, #15829, #5970, .T. ) ;
#2855 = ORIENTED_EDGE ( 'NONE', *, *, #8486, .T. ) ;
#2856 = AXIS2_PLACEMENT_3D ( 'NONE', #10060, #16162, #13432 ) ;
#2857 = CARTESIAN_POINT ( 'NONE',  ( 13.00000000000000533, -5.207209108562836697, 2.318398865532038666 ) ) ;
#2858 = CARTESIAN_POINT ( 'NONE',  ( -1.800000000000000488, 5.143516556418882928E-16, 4.200000000000000178 ) ) ;
#2859 = VERTEX_POINT ( 'NONE', #345 ) ;
#2860 = DIRECTION ( 'NONE',  ( 0.000000000000000000, 0.000000000000000000, -1.000000000000000000 ) ) ;
#2861 = DIRECTION ( 'NONE',  ( 0.000000000000000000, 0.000000000000000000, -1.000000000000000000 ) ) ;
#2862 = ORIENTED_EDGE ( 'NONE', *, *, #7351, .F. ) ;
#2863 = DIRECTION ( 'NONE',  ( -0.000000000000000000, 0.8660254037844329345, 0.5000000000000097700 ) ) ;
#2864 = EDGE_CURVE ( 'NONE', #6786, #11375, #13861, .T. ) ;
#2865 = CARTESIAN_POINT ( 'NONE',  ( 9.343749997951615427, 3.499494075959816541, -3.499494075959816541 ) ) ;
#2866 = DIRECTION ( 'NONE',  ( 1.000000000000000000, 0.000000000000000000, 0.000000000000000000 ) ) ;
#2867 = EDGE_LOOP ( 'NONE', ( #6580, #7697, #16472, #2187 ) ) ;
#2868 = DIRECTION ( 'NONE',  ( -1.000000000000000000, 0.000000000000000000, 0.000000000000000000 ) ) ;
#2869 = AXIS2_PLACEMENT_3D ( 'NONE', #10122, #16222, #3911 ) ;
#2870 = DIRECTION ( 'NONE',  ( 0.000000000000000000, 0.000000000000000000, -1.000000000000000000 ) ) ;
#2871 = ORIENTED_EDGE ( 'NONE', *, *, #19538, .F. ) ;
#2872 = CARTESIAN_POINT ( 'NONE',  ( 15.19790265903627358, 9.644882309621939598, -32.00000000000000000 ) ) ;
#2873 = ADVANCED_FACE ( 'NONE', ( #3246 ), #6333, .T. ) ;
#2874 = FACE_OUTER_BOUND ( 'NONE', #4273, .T. ) ;
#2875 = LINE ( 'NONE', #5771, #17263 ) ;
#2876 = CARTESIAN_POINT ( 'NONE',  ( 4.942249507334556036, -0.2590123213421313686, -9.968749997951615427 ) ) ;
#2877 = CARTESIAN_POINT ( 'NONE',  ( -5.763142191869152775, 0.3020334839683282979, -10.81249999590322375 ) ) ;
#2878 = ORIENTED_EDGE ( 'NONE', *, *, #16462, .T. ) ;
#2879 = DIRECTION ( 'NONE',  ( 0.000000000000000000, 0.000000000000000000, -1.000000000000000000 ) ) ;
#2880 = DIRECTION ( 'NONE',  ( 1.000000000000000000, 0.000000000000000000, 0.000000000000000000 ) ) ;
#2881 = CIRCLE ( 'NONE', #14068, 0.03079999999999923077 ) ;
#2882 = EDGE_LOOP ( 'NONE', ( #8062, #11799, #2714, #19306 ) ) ;
#2883 = B_SPLINE_CURVE_WITH_KNOTS ( 'NONE', 3,
 ( #8110, #14219, #5208, #17221, #6301, #12525 ),
 .UNSPECIFIED., .F., .F.,
 ( 4, 2, 4 ),
 ( 2.321268216997094965E-07, 0.001878622960950492287, 0.003757013795079284547 ),
 .UNSPECIFIED. ) ;
#2884 = CARTESIAN_POINT ( 'NONE',  ( 12.84374999795161543, -3.632567103900546712, 3.270778111535314281 ) ) ;
#2885 = AXIS2_PLACEMENT_3D ( 'NONE', #9936, #2116, #726 ) ;
#2886 = DIRECTION ( 'NONE',  ( 1.000000000000000000, 0.000000000000000000, 0.000000000000000000 ) ) ;
#2887 = CARTESIAN_POINT ( 'NONE',  ( 11.46874999795161543, 2.444050593750049405, -4.233219804643852946 ) ) ;
#2888 = DIRECTION ( 'NONE',  ( 0.000000000000000000, 0.000000000000000000, 1.000000000000000000 ) ) ;
#2889 = EDGE_CURVE ( 'NONE', #123, #9264, #1754, .T. ) ;
#2890 = ORIENTED_EDGE ( 'NONE', *, *, #4836, .T. ) ;
#2891 = PLANE ( 'NONE',  #3067 ) ;
#2892 = DIRECTION ( 'NONE',  ( 1.000000000000000000, 0.000000000000000000, 0.000000000000000000 ) ) ;
#2893 = CARTESIAN_POINT ( 'NONE',  ( -0.5958122406255597081, 5.668774803599165857, -15.31249999590322552 ) ) ;
#2894 = ORIENTED_EDGE ( 'NONE', *, *, #1008, .T. ) ;
#2895 = DIRECTION ( 'NONE',  ( -1.000000000000000000, -0.000000000000000000, -0.000000000000000000 ) ) ;
#2896 = DIRECTION ( 'NONE',  ( 0.000000000000000000, 0.000000000000000000, 1.000000000000000000 ) ) ;
#2897 = EDGE_CURVE ( 'NONE', #13172, #11527, #18553, .T. ) ;
#2898 = DIRECTION ( 'NONE',  ( 1.000000000000000000, 0.000000000000000000, 0.000000000000000000 ) ) ;
#2899 = DIRECTION ( 'NONE',  ( 1.000000000000000000, 0.000000000000000000, 0.000000000000000000 ) ) ;
#2900 = DIRECTION ( 'NONE',  ( 1.000000000000000000, 0.000000000000000000, 0.000000000000000000 ) ) ;
#2901 = VERTEX_POINT ( 'NONE', #6628 ) ;
#2902 = CYLINDRICAL_SURFACE ( 'NONE', #4530, 13.19999999999999929 ) ;
#2903 = CARTESIAN_POINT ( 'NONE',  ( 1.039999999999995817, 27.76164181293051669, 4.147968289691385202 ) ) ;
#2904 = VERTEX_POINT ( 'NONE', #7020 ) ;
#2905 = AXIS2_PLACEMENT_3D ( 'NONE', #15793, #8184, #13348 ) ;
#2906 = CIRCLE ( 'NONE', #4206, 8.000000000000000000 ) ;
#2907 = DIRECTION ( 'NONE',  ( 1.000000000000000000, 0.000000000000000000, 0.000000000000000000 ) ) ;
#2908 = LINE ( 'NONE', #118, #4553 ) ;
#2909 = EDGE_LOOP ( 'NONE', ( #185, #12171, #12080, #172, #15264, #17631, #15717, #16655 ) ) ;
#2910 = CARTESIAN_POINT ( 'NONE',  ( -1.773574444220725077, 4.620319390059829168, -6.968749997951614539 ) ) ;
#2911 = CARTESIAN_POINT ( 'NONE',  ( 15.31249999590322552, -2.318398865532073305, 5.207209108562820710 ) ) ;
#2912 = ORIENTED_EDGE ( 'NONE', *, *, #2271, .F. ) ;
#2913 = CARTESIAN_POINT ( 'NONE',  ( 0.02436607992776325046, -24.15498966839958683, -5.391175441198872598 ) ) ;
#2914 = ORIENTED_EDGE ( 'NONE', *, *, #2598, .F. ) ;
#2915 = B_SPLINE_CURVE_WITH_KNOTS ( 'NONE', 3,
 ( #2070, #15981, #15683, #8069 ),
 .UNSPECIFIED., .F., .F.,
 ( 4, 4 ),
 ( 0.005258110598983609975, 0.005948376585272729597 ),
 .UNSPECIFIED. ) ;
#2916 = CARTESIAN_POINT ( 'NONE',  ( -7.289885936478958328, -4.956617915597525403, -0.4930775504667679332 ) ) ;
#2917 = EDGE_LOOP ( 'NONE', ( #17953, #13648 ) ) ;
#2918 = B_SPLINE_CURVE_WITH_KNOTS ( 'NONE', 3,
 ( #1601, #507, #1994, #7692 ),
 .UNSPECIFIED., .F., .F.,
 ( 4, 4 ),
 ( 2.135345996541640089E-07, 0.0006888010880211291841 ),
 .UNSPECIFIED. ) ;
#2919 = CARTESIAN_POINT ( 'NONE',  ( 3.954556930911861112, 2.873153789725825913, -14.46874999795161720 ) ) ;
#2920 = EDGE_CURVE ( 'NONE', #3846, #1264, #10961, .T. ) ;
#2921 = CARTESIAN_POINT ( 'NONE',  ( 2.179781338987520467, -23.94322454545470436, 12.96989951879399072 ) ) ;
#2922 = CARTESIAN_POINT ( 'NONE',  ( 2.647025296875021638, 4.584782303107579615, -7.078124996927420476 ) ) ;
#2923 = CARTESIAN_POINT ( 'NONE',  ( 10.96874999795161720, -3.114526743279228072, -3.846120219227966430 ) ) ;
#2924 = VECTOR ( 'NONE', #15921, 1000.000000000000227 ) ;
#2925 = AXIS2_PLACEMENT_3D ( 'NONE', #7500, #7391, #1216 ) ;
#2926 = CARTESIAN_POINT ( 'NONE',  ( 12.73273607671833929, 0.6164700669140775746, 4.866269517993460525 ) ) ;
#2927 = ORIENTED_EDGE ( 'NONE', *, *, #18222, .F. ) ;
#2928 = AXIS2_PLACEMENT_3D ( 'NONE', #14727, #19714, #14823 ) ;
#2929 = FACE_OUTER_BOUND ( 'NONE', #10183, .T. ) ;
#2930 = DIRECTION ( 'NONE',  ( 0.8090169943749512260, 0.5877852522924679191, 0.000000000000000000 ) ) ;
#2931 = ORIENTED_EDGE ( 'NONE', *, *, #873, .T. ) ;
#2932 = DIRECTION ( 'NONE',  ( 1.000000000000000000, 0.000000000000000000, 0.000000000000000000 ) ) ;
#2933 = ADVANCED_FACE ( 'NONE', ( #559, #3747 ), #6928, .T. ) ;
#2934 = DIRECTION ( 'NONE',  ( 0.000000000000000000, 0.000000000000000000, -1.000000000000000000 ) ) ;
#2935 = ORIENTED_EDGE ( 'NONE', *, *, #12271, .F. ) ;
#2936 = VECTOR ( 'NONE', #17518, 1000.000000000000000 ) ;
#2937 = DIRECTION ( 'NONE',  ( -1.000000000000000000, 0.000000000000000000, -0.000000000000000000 ) ) ;
#2938 = CIRCLE ( 'NONE', #11266, 2.524999999999995914 ) ;
#2939 = DIRECTION ( 'NONE',  ( -0.000000000000000000, -0.000000000000000000, 1.000000000000000000 ) ) ;
#2940 = AXIS2_PLACEMENT_3D ( 'NONE', #14995, #13486, #2481 ) ;
#2941 = CARTESIAN_POINT ( 'NONE',  ( 2.789999999999999147, 22.71065055754465689, -9.836394144775473691 ) ) ;
#2942 = ORIENTED_EDGE ( 'NONE', *, *, #1205, .F. ) ;
#2943 = PLANE ( 'NONE',  #14850 ) ;
#2944 = EDGE_CURVE ( 'NONE', #12101, #5745, #3928, .T. ) ;
#2945 = EDGE_LOOP ( 'NONE', ( #5707, #1193, #1893, #387 ) ) ;
#2946 = DIRECTION ( 'NONE',  ( -0.000000000000000000, -0.000000000000000000, -1.000000000000000000 ) ) ;
#2947 = CARTESIAN_POINT ( 'NONE',  ( 13.32184790671640151, 13.12143529358541016, 32.00000000000000000 ) ) ;
#2948 = CARTESIAN_POINT ( 'NONE',  ( -3.814044456245531567, -4.235925505221111997, -11.31249999590322375 ) ) ;
#2949 = ORIENTED_EDGE ( 'NONE', *, *, #1019, .F. ) ;
#2950 =( BOUNDED_SURFACE ( )  B_SPLINE_SURFACE ( 1, 2, ( 
 ( #15739, #9748, #634, #9848, #12833, #6408, #4932, #15838, #14035, #5026, #14335, #6709, #11036, #11340, #17439, #15938, #9542 ),
 ( #15543, #15639, #2221, #13940, #8018, #329, #1925, #232, #2027, #434, #6511, #12640, #10939, #17044, #11137, #6316, #3333 ) ),
 .UNSPECIFIED., .F., .F., .F. ) 
 B_SPLINE_SURFACE_WITH_KNOTS ( ( 2, 2 ),
 ( 3, 2, 2, 2, 2, 2, 2, 2, 3 ),
 ( 0.000000000000000000, 1.000000000000000000 ),
 ( 0.000000000000000000, 0.05000000000000000278, 0.1000000000000000056, 0.1499999999999999944, 0.2000000000000000111, 0.2500000000000000000, 0.2999999999999999889, 0.3499999999999999778, 0.4000000000000000222 ),
 .UNSPECIFIED. ) 
 GEOMETRIC_REPRESENTATION_ITEM ( )  RATIONAL_B_SPLINE_SURFACE ( (
 ( 1.000000000000000000, 0.9876883405951377704, 1.000000000000000000, 0.9876883405951377704, 1.000000000000000000, 0.9876883405951377704, 1.000000000000000000, 0.9876883405951377704, 1.000000000000000000, 0.9876883405951377704, 1.000000000000000000, 0.9876883405951377704, 1.000000000000000000, 0.9876883405951377704, 1.000000000000000000, 0.9876883405951377704, 1.000000000000000000),
 ( 1.000000000000000000, 0.9876883405951377704, 1.000000000000000000, 0.9876883405951377704, 1.000000000000000000, 0.9876883405951377704, 1.000000000000000000, 0.9876883405951377704, 1.000000000000000000, 0.9876883405951377704, 1.000000000000000000, 0.9876883405951377704, 1.000000000000000000, 0.9876883405951377704, 1.000000000000000000, 0.9876883405951377704, 1.000000000000000000) ) ) 
 REPRESENTATION_ITEM ( '' )  SURFACE ( )  );
#2951 = EDGE_LOOP ( 'NONE', ( #1493, #13570, #18839, #2548, #13326, #16612 ) ) ;
#2952 = EDGE_CURVE ( 'NONE', #5462, #12828, #11482, .T. ) ;
#2953 = DIRECTION ( 'NONE',  ( -0.000000000000000000, -0.000000000000000000, 1.000000000000000000 ) ) ;
#2954 = DIRECTION ( 'NONE',  ( 0.000000000000000000, 0.000000000000000000, 1.000000000000000000 ) ) ;
#2955 = EDGE_LOOP ( 'NONE', ( #4427, #15410, #16999, #3356 ) ) ;
#2956 = AXIS2_PLACEMENT_3D ( 'NONE', #1273, #5960, #7558 ) ;
#2957 = CARTESIAN_POINT ( 'NONE',  ( 1.749999999999998002, -27.76164181293049182, -4.147968289691579713 ) ) ;
#2958 = ORIENTED_EDGE ( 'NONE', *, *, #16901, .F. ) ;
#2959 = CARTESIAN_POINT ( 'NONE',  ( -10.58013454126452224, -14.56230589874905235, 35.00000000000000000 ) ) ;
#2960 = AXIS2_PLACEMENT_3D ( 'NONE', #16752, #10085, #15047 ) ;
#2961 = EDGE_CURVE ( 'NONE', #17554, #3802, #14354, .T. ) ;
#2962 = VERTEX_POINT ( 'NONE', #19147 ) ;
#2963 = CIRCLE ( 'NONE', #9694, 24.12539914357697413 ) ;
#2964 =( GEOMETRIC_REPRESENTATION_CONTEXT ( 3 ) GLOBAL_UNCERTAINTY_ASSIGNED_CONTEXT ( ( #14797 ) ) GLOBAL_UNIT_ASSIGNED_CONTEXT ( ( #9869, #16161, #8249 ) ) REPRESENTATION_CONTEXT ( 'NONE', 'WORKASPACE' ) );
#2965 = MANIFOLD_SOLID_BREP ( 'BaseBody', #15109 ) ;
#2966 = ADVANCED_FACE ( 'NONE', ( #13144 ), #17459, .F. ) ;
#2967 = FACE_OUTER_BOUND ( 'NONE', #15097, .T. ) ;
#2968 = FACE_OUTER_BOUND ( 'NONE', #16182, .T. ) ;
#2969 = CARTESIAN_POINT ( 'NONE',  ( -0.5109457054261112852, 4.861323657744413218, -14.84374999795161543 ) ) ;
#2970 = AXIS2_PLACEMENT_3D ( 'NONE', #8264, #6744, #13554 ) ;
#2971 = ORIENTED_EDGE ( 'NONE', *, *, #9449, .T. ) ;
#2972 = DIRECTION ( 'NONE',  ( -1.000000000000000000, -6.419766481290786633E-33, 0.000000000000000000 ) ) ;
#2973 = FILL_AREA_STYLE ('',( #16390 ) ) ;
#2974 = ORIENTED_EDGE ( 'NONE', *, *, #12220, .F. ) ;
#2975 = CARTESIAN_POINT ( 'NONE',  ( 14.00000000000000178, 1.714505518806294835E-15, 35.00000000000000000 ) ) ;
#2976 = CARTESIAN_POINT ( 'NONE',  ( 0.000000000000000000, 23.48180575137729775, 5.535312321042836103 ) ) ;
#2977 = AXIS2_PLACEMENT_3D ( 'NONE', #2614, #4029, #16150 ) ;
#2978 = DIRECTION ( 'NONE',  ( -0.000000000000000000, -0.000000000000000000, -1.000000000000000000 ) ) ;
#2979 = AXIS2_PLACEMENT_3D ( 'NONE', #7261, #5294, #11400 ) ;
#2980 = DIRECTION ( 'NONE',  ( 0.000000000000000000, 0.000000000000000000, 1.000000000000000000 ) ) ;
#2981 = CARTESIAN_POINT ( 'NONE',  ( 2.873153789725825025, 3.954556930911862000, -13.84374999795161543 ) ) ;
#2982 = VERTEX_POINT ( 'NONE', #8149 ) ;
#2983 = DIRECTION ( 'NONE',  ( 0.000000000000000000, 0.000000000000000000, -1.000000000000000000 ) ) ;
#2984 = ADVANCED_FACE ( 'NONE', ( #4041 ), #18155, .F. ) ;
#2985 = DIRECTION ( 'NONE',  ( -1.000000000000000000, -0.000000000000000000, -0.000000000000000000 ) ) ;
#2986 = MECHANICAL_DESIGN_GEOMETRIC_PRESENTATION_REPRESENTATION (  '', ( #15452 ), #6485 ) ;
#2987 = VERTEX_POINT ( 'NONE', #7694 ) ;
#2988 = CARTESIAN_POINT ( 'NONE',  ( 8.343749997951611874, 2.695436003842704764, 4.150607464521812062 ) ) ;
#2989 = CYLINDRICAL_SURFACE ( 'NONE', #673, 3.000000000000000000 ) ;
#2990 = CIRCLE ( 'NONE', #9390, 2.524999999999995914 ) ;
#2991 = DIRECTION ( 'NONE',  ( 0.000000000000000000, 0.000000000000000000, 1.000000000000000000 ) ) ;
#2992 = CARTESIAN_POINT ( 'NONE',  ( 2.789999999999999147, 24.34211360614300190, 7.909232158574900140 ) ) ;
#2993 = VERTEX_POINT ( 'NONE', #7594 ) ;
#2994 = DIRECTION ( 'NONE',  ( -1.000000000000000000, -0.000000000000000000, -0.000000000000000000 ) ) ;
#2995 = DIRECTION ( 'NONE',  ( 1.000000000000000000, 0.000000000000000000, 0.000000000000000000 ) ) ;
#2996 = ORIENTED_EDGE ( 'NONE', *, *, #13252, .F. ) ;
#2997 = DIRECTION ( 'NONE',  ( 1.000000000000000000, 0.000000000000000000, 0.000000000000000000 ) ) ;
#2998 = AXIS2_PLACEMENT_3D ( 'NONE', #16100, #2379, #8493 ) ;
#2999 = CARTESIAN_POINT ( 'NONE',  ( 2.604434514863826156, 10.67816411292164958, 23.63475234378986300 ) ) ;
#3000 = B_SPLINE_CURVE_WITH_KNOTS ( 'NONE', 3,
 ( #5622, #2429, #17839, #13047 ),
 .UNSPECIFIED., .F., .F.,
 ( 4, 4 ),
 ( 1.981826382900813409E-07, 0.0006887856082032195850 ),
 .UNSPECIFIED. ) ;
#3001 = CARTESIAN_POINT ( 'NONE',  ( 11.96874999795161365, -4.888101187499994893, -0.7741991708319226895 ) ) ;
#3002 = CARTESIAN_POINT ( 'NONE',  ( 14.34374999795161365, 3.499494075959816541, 3.499494075959815653 ) ) ;
#3003 = CARTESIAN_POINT ( 'NONE',  ( 2.765633920072234631, 16.37294372382885044, -18.55949924794875017 ) ) ;
#3004 = LINE ( 'NONE', #9119, #3451 ) ;
#3005 = ORIENTED_EDGE ( 'NONE', *, *, #2295, .F. ) ;
#3006 = EDGE_CURVE ( 'NONE', #6920, #8766, #7103, .T. ) ;
#3007 = AXIS2_PLACEMENT_3D ( 'NONE', #18946, #15852, #749 ) ;
#3008 = CARTESIAN_POINT ( 'NONE',  ( -4.780397808154247308, 1.280903732194486722, -13.96874999795161365 ) ) ;
#3009 = DIRECTION ( 'NONE',  ( 0.000000000000000000, 1.000000000000000000, -1.224646799147353207E-16 ) ) ;
#3010 = ORIENTED_EDGE ( 'NONE', *, *, #19158, .T. ) ;
#3011 = CIRCLE ( 'NONE', #14202, 1.000000000000000888 ) ;
#3012 = EDGE_CURVE ( 'NONE', #10657, #6388, #9214, .T. ) ;
#3013 = CARTESIAN_POINT ( 'NONE',  ( 17.68117051311639898, -3.372863662543048591, -35.00000000000000000 ) ) ;
#3014 = CARTESIAN_POINT ( 'NONE',  ( 2.873153789725797491, -3.954556930911881985, -9.843749997951615427 ) ) ;
#3015 = ORIENTED_EDGE ( 'NONE', *, *, #12236, .T. ) ;
#3016 = CARTESIAN_POINT ( 'NONE',  ( 9.343749997951615427, 4.780397808154257078, 1.280903732194454081 ) ) ;
#3017 = CARTESIAN_POINT ( 'NONE',  ( -2.873153789725825469, 3.954556930911862000, -9.468749997951615427 ) ) ;
#3018 = AXIS2_PLACEMENT_3D ( 'NONE', #16840, #1725, #7815 ) ;
#3019 = VERTEX_POINT ( 'NONE', #6092 ) ;
#3020 = CARTESIAN_POINT ( 'NONE',  ( 0.5321745407694743468, -26.58873630738047922, -4.993157874728098022 ) ) ;
#3021 = EDGE_LOOP ( 'NONE', ( #9314, #6274, #5228, #2146, #136, #12210 ) ) ;
#3022 = EDGE_LOOP ( 'NONE', ( #7553, #18998, #8944, #1153, #18070, #8036, #3399, #18429, #14732, #16328, #6534, #7883, #9284, #10530, #3417, #782, #10195 ) ) ;
#3023 = ADVANCED_FACE ( 'NONE', ( #13711 ), #15412, .F. ) ;
#3024 = FACE_OUTER_BOUND ( 'NONE', #11731, .T. ) ;
#3025 = FACE_OUTER_BOUND ( 'NONE', #3657, .T. ) ;
#3026 = CARTESIAN_POINT ( 'NONE',  ( 9.968749997951617203, -4.150607464521772094, -2.695436003842760275 ) ) ;
#3027 = AXIS2_PLACEMENT_3D ( 'NONE', #12052, #18154, #6128 ) ;
#3028 = CARTESIAN_POINT ( 'NONE',  ( 12.46874999795161543, 1.016293382781411792, 4.781284448697194378 ) ) ;
#3029 = ORIENTED_EDGE ( 'NONE', *, *, #2426, .F. ) ;
#3030 = CARTESIAN_POINT ( 'NONE',  ( 15.19790265903627358, 9.644882309621939598, -35.00000000000000000 ) ) ;
#3031 = CARTESIAN_POINT ( 'NONE',  ( 2.999999999999998224, 0.000000000000000000, 0.000000000000000000 ) ) ;
#3032 = B_SPLINE_CURVE_WITH_KNOTS ( 'NONE', 3,
 ( #13683, #7565, #4181, #7256 ),
 .UNSPECIFIED., .F., .F.,
 ( 4, 4 ),
 ( 0.005258110598983608240, 0.005948376585272733066 ),
 .UNSPECIFIED. ) ;
#3033 = VERTEX_POINT ( 'NONE', #7797 ) ;
#3034 = EDGE_CURVE ( 'NONE', #18102, #11367, #14166, .T. ) ;
#3035 = DIRECTION ( 'NONE',  ( 0.000000000000000000, 0.000000000000000000, 1.000000000000000000 ) ) ;
#3036 = DIRECTION ( 'NONE',  ( 0.000000000000000000, 0.000000000000000000, 1.000000000000000000 ) ) ;
#3037 = VERTEX_POINT ( 'NONE', #10150 ) ;
#3038 = VECTOR ( 'NONE', #658, 1000.000000000000000 ) ;
#3039 = CARTESIAN_POINT ( 'NONE',  ( -1.800000000000000488, 0.000000000000000000, 0.000000000000000000 ) ) ;
#3041 = DIRECTION ( 'NONE',  ( 0.000000000000000000, 0.000000000000000000, -1.000000000000000000 ) ) ;
#3040 = AXIS2_PLACEMENT_3D ( 'NONE', #3783, #14505, #9999 ) ;
#3042 = B_SPLINE_CURVE_WITH_KNOTS ( 'NONE', 3,
 ( #5003, #8202, #3892, #2390, #3796, #11207 ),
 .UNSPECIFIED., .F., .F.,
 ( 4, 2, 4 ),
 ( 4.462636682233640623E-07, 0.001879885020955585333, 0.003759323778242947261 ),
 .UNSPECIFIED. ) ;
#3043 = SURFACE_STYLE_FILL_AREA ( #6799 ) ;
#3044 = ORIENTED_EDGE ( 'NONE', *, *, #14676, .T. ) ;
#3045 = CARTESIAN_POINT ( 'NONE',  ( 9.968749997951615427, -4.150607464521772094, -2.695436003842760719 ) ) ;
#3046 = ORIENTED_EDGE ( 'NONE', *, *, #13258, .T. ) ;
#3047 = CARTESIAN_POINT ( 'NONE',  ( 0.000000000000000000, 0.000000000000000000, 0.000000000000000000 ) ) ;
#3048 = DIRECTION ( 'NONE',  ( 0.8660254037844432595, 0.4999999999999920619, -0.000000000000000000 ) ) ;
#3049 = CARTESIAN_POINT ( 'NONE',  ( -5.575441324182703440, -1.185096637661177343, -13.31249999590322730 ) ) ;
#3050 = VERTEX_POINT ( 'NONE', #10713 ) ;
#3051 = ORIENTED_EDGE ( 'NONE', *, *, #14724, .T. ) ;
#3052 = CARTESIAN_POINT ( 'NONE',  ( 0.1855657389739081564, 25.39738473785008210, -5.253342437939463316 ) ) ;
#3053 = CARTESIAN_POINT ( 'NONE',  ( 4.936344801571308061, 2.849999999999989875, -12.31249999590322552 ) ) ;
#3054 = ORIENTED_EDGE ( 'NONE', *, *, #14618, .T. ) ;
#3055 = EDGE_CURVE ( 'NONE', #16700, #1129, #12317, .T. ) ;
#3056 = CARTESIAN_POINT ( 'NONE',  ( 0.000000000000000000, 0.000000000000000000, -30.00000000000000355 ) ) ;
#3057 = ORIENTED_EDGE ( 'NONE', *, *, #12490, .F. ) ;
#3058 = AXIS2_PLACEMENT_3D ( 'NONE', #16675, #18273, #13460 ) ;
#3059 = DIRECTION ( 'NONE',  ( 0.000000000000000000, 0.000000000000000000, 1.000000000000000000 ) ) ;
#3060 = ADVANCED_FACE ( 'NONE', ( #6286 ), #12413, .T. ) ;
#3061 = ORIENTED_EDGE ( 'NONE', *, *, #3062, .T. ) ;
#3062 = EDGE_CURVE ( 'NONE', #7744, #1573, #11925, .T. ) ;
#3063 = CARTESIAN_POINT ( 'NONE',  ( -22.00000000000000355, 2.694222958124177204E-15, 35.00000000000000000 ) ) ;
#3064 = CARTESIAN_POINT ( 'NONE',  ( -1.869200000000000195, 0.000000000000000000, 0.000000000000000000 ) ) ;
#3065 =( BOUNDED_CURVE ( )  B_SPLINE_CURVE ( 2, ( #7755, #14363, #12763, #6838, #8155, #463, #14056, #566, #14262, #12861, #6536, #11366, #6635, #14466, #659 ),
 .UNSPECIFIED., .F., .F. ) 
 B_SPLINE_CURVE_WITH_KNOTS ( ( 3, 2, 2, 2, 2, 2, 2, 3 ),
 ( 0.000000000000000000, 0.05000000000000000278, 0.1000000000000000056, 0.1499999999999999944, 0.2000000000000000111, 0.2500000000000000000, 0.2999999999999999889, 0.3265529187307101844 ),
 .UNSPECIFIED. ) 
 CURVE ( )  GEOMETRIC_REPRESENTATION_ITEM ( )  RATIONAL_B_SPLINE_CURVE ( ( 1.000000000000000000, 0.9876883405951377704, 1.000000000000000000, 0.9876883405951377704, 1.000000000000000000, 0.9876883405951377704, 1.000000000000000000, 0.9876883405951377704, 1.000000000000000000, 0.9876883405951377704, 1.000000000000000000, 0.9876883405951377704, 1.000000000000000000, 0.9934617901676502383, 0.9938679225082089896 ) ) 
 REPRESENTATION_ITEM ( '' )  );
#3066 = CARTESIAN_POINT ( 'NONE',  ( 5.699999999999994849, -0.9027913098498966393, -7.812499995903224637 ) ) ;
#3067 = AXIS2_PLACEMENT_3D ( 'NONE', #10511, #19606, #13503 ) ;
#3068 = ORIENTED_EDGE ( 'NONE', *, *, #16920, .F. ) ;
#3069 = VERTEX_POINT ( 'NONE', #8739 ) ;
#3070 = DIRECTION ( 'NONE',  ( 1.000000000000000000, 0.000000000000000000, 0.000000000000000000 ) ) ;
#3071 = DIRECTION ( 'NONE',  ( 1.000000000000000000, 0.000000000000000000, 0.000000000000000000 ) ) ;
#3072 = VECTOR ( 'NONE', #3207, 1000.000000000000000 ) ;
#3073 = VERTEX_POINT ( 'NONE', #2626 ) ;
#3074 = CARTESIAN_POINT ( 'NONE',  ( -2.000000000000000000, -2.000000000000001776, 37.99999999999999289 ) ) ;
#3075 = FACE_BOUND ( 'NONE', #16640, .T. ) ;
#3076 = CARTESIAN_POINT ( 'NONE',  ( 2.765633920072239071, -16.37294372382844543, -18.55949924794910544 ) ) ;
#3077 = DIRECTION ( 'NONE',  ( -0.000000000000000000, -0.000000000000000000, 1.000000000000000000 ) ) ;
#3078 = CARTESIAN_POINT ( 'NONE',  ( -2.000000000000001776, 9.184850993605147944E-16, -7.500000000000000000 ) ) ;
#3079 = ORIENTED_EDGE ( 'NONE', *, *, #11485, .F. ) ;
#3080 = CARTESIAN_POINT ( 'NONE',  ( -2.602085213965210642E-14, -9.165435523385315975, -0.7089489049740167470 ) ) ;
#3081 = CARTESIAN_POINT ( 'NONE',  ( 12.66727757604273386, -4.360680574150373717E-16, 5.700000000000001066 ) ) ;
#3082 = AXIS2_PLACEMENT_3D ( 'NONE', #10000, #14196, #16102 ) ;
#3083 = ORIENTED_EDGE ( 'NONE', *, *, #17542, .F. ) ;
#3084 = CARTESIAN_POINT ( 'NONE',  ( 0.02436607992776238310, -2.336989772644097574, -24.63872515616085224 ) ) ;
#3085 = CIRCLE ( 'NONE', #14277, 3.000000000000000000 ) ;
#3086 = ADVANCED_FACE ( 'NONE', ( #18218 ), #18506, .T. ) ;
#3087 = EDGE_CURVE ( 'NONE', #14880, #4759, #6473, .T. ) ;
#3088 = CARTESIAN_POINT ( 'NONE',  ( 14.86923836996420434, -11.47363181547641453, 35.00000000000000000 ) ) ;
#3089 = CARTESIAN_POINT ( 'NONE',  ( 7.968749997951616315, -2.695436003842674122, -4.150607464521828938 ) ) ;
#3090 = DIRECTION ( 'NONE',  ( -1.000000000000000000, 0.000000000000000000, 0.000000000000000000 ) ) ;
#3091 = ORIENTED_EDGE ( 'NONE', *, *, #7862, .F. ) ;
#3092 = CARTESIAN_POINT ( 'NONE',  ( 12.00000000000000533, 5.421022142882376826, 1.761396867937200073 ) ) ;
#3093 = SURFACE_STYLE_USAGE ( .BOTH. , #4601 ) ;
#3094 = DIRECTION ( 'NONE',  ( -0.000000000000000000, -0.000000000000000000, 1.000000000000000000 ) ) ;
#3095 = EDGE_CURVE ( 'NONE', #6790, #1120, #13387, .T. ) ;
#3096 = FACE_OUTER_BOUND ( 'NONE', #17023, .T. ) ;
#3097 = VERTEX_POINT ( 'NONE', #701 ) ;
#3098 = CARTESIAN_POINT ( 'NONE',  ( 0.000000000000000000, 4.200000000000000178, -28.99999999999999645 ) ) ;
#3099 = CIRCLE ( 'NONE', #14287, 24.12539914357697768 ) ;
#3100 = CARTESIAN_POINT ( 'NONE',  ( -90.00000000000000000, 0.000000000000000000, 0.000000000000000000 ) ) ;
#3101 = CARTESIAN_POINT ( 'NONE',  ( 9.500000000000003553, 4.840010801796480244, 3.143139765844623401 ) ) ;
#3102 = AXIS2_PLACEMENT_3D ( 'NONE', #13384, #19483, #2772 ) ;
#3103 = CARTESIAN_POINT ( 'NONE',  ( 12.34374999795161543, 4.888101187500000222, 0.7741991708318884946 ) ) ;
#3104 = ORIENTED_EDGE ( 'NONE', *, *, #4560, .T. ) ;
#3105 = CARTESIAN_POINT ( 'NONE',  ( -41.99999999999999289, 1.999999999999998224, -2.000000000000000000 ) ) ;
#3106 = EDGE_CURVE ( 'NONE', #16740, #11695, #1703, .T. ) ;
#3107 = CARTESIAN_POINT ( 'NONE',  ( -4.366025403784388637, -7.562177826491097044, 41.99999999999999289 ) ) ;
#3108 = EDGE_CURVE ( 'NONE', #6978, #16213, #14302, .T. ) ;
#3109 = EDGE_LOOP ( 'NONE', ( #14326, #16621 ) ) ;
#3110 = CARTESIAN_POINT ( 'NONE',  ( 7.468749997951615427, -1.510506337161893864, 4.648860486681943627 ) ) ;
#3111 = CARTESIAN_POINT ( 'NONE',  ( -1.001543065824775120E-15, -9.165435523385328409, -6.527800000000000047 ) ) ;
#3112 = ORIENTED_EDGE ( 'NONE', *, *, #3156, .T. ) ;
#3113 = VECTOR ( 'NONE', #17109, 1000.000000000000114 ) ;
#3114 = AXIS2_PLACEMENT_3D ( 'NONE', #17305, #7895, #1998 ) ;
#3115 = CARTESIAN_POINT ( 'NONE',  ( 0.000000000000000000, 0.000000000000000000, 0.000000000000000000 ) ) ;
#3116 = CARTESIAN_POINT ( 'NONE',  ( 3.499494075959792116, -3.499494075959840966, -9.343749997951615427 ) ) ;
#3117 = VERTEX_POINT ( 'NONE', #3401 ) ;
#3118 = DIRECTION ( 'NONE',  ( 1.000000000000000000, 0.000000000000000000, 0.000000000000000000 ) ) ;
#3119 = CARTESIAN_POINT ( 'NONE',  ( 0.5279272304333949561, 24.43806413951675793, 11.57956866523226580 ) ) ;
#3120 = ADVANCED_FACE ( 'NONE', ( #18799 ), #3498, .F. ) ;
#3121 = ORIENTED_EDGE ( 'NONE', *, *, #16030, .T. ) ;
#3122 = CARTESIAN_POINT ( 'NONE',  ( 0.000000000000000000, 0.000000000000000000, -6.000000000000005329 ) ) ;
#3123 = VERTEX_POINT ( 'NONE', #12904 ) ;
#3124 = LINE ( 'NONE', #1433, #16854 ) ;
#3125 = ORIENTED_EDGE ( 'NONE', *, *, #3539, .F. ) ;
#3126 = CARTESIAN_POINT ( 'NONE',  ( 2.789999999999999147, -18.55949924794880346, -16.37294372382878649 ) ) ;
#3127 = CYLINDRICAL_SURFACE ( 'NONE', #8024, 1.000000000000003553 ) ;
#3128 = CARTESIAN_POINT ( 'NONE',  ( -1.886022603841227552, 0.000000000000000000, 0.000000000000000000 ) ) ;
#3129 = CIRCLE ( 'NONE', #14318, 2.524999999999995914 ) ;
#3130 = ADVANCED_FACE ( 'NONE', ( #7892 ), #14100, .F. ) ;
#3131 = CARTESIAN_POINT ( 'NONE',  ( 2.789999999999999147, 18.55949924794916228, -16.37294372382838148 ) ) ;
#3132 = EDGE_CURVE ( 'NONE', #5629, #6948, #13522, .T. ) ;
#3133 = VECTOR ( 'NONE', #19416, 1000.000000000000000 ) ;
#3134 = EDGE_LOOP ( 'NONE', ( #10248, #14667 ) ) ;
#3135 = DIRECTION ( 'NONE',  ( -1.000000000000000000, 0.000000000000000000, 0.000000000000000000 ) ) ;
#3136 = MANIFOLD_SOLID_BREP ( 'InnerRace', #13872 ) ;
#3137 = CARTESIAN_POINT ( 'NONE',  ( -19.00000000000000355, 3.278623949159158890, 2.625000000000000888 ) ) ;
#3138 = VERTEX_POINT ( 'NONE', #18698 ) ;
#3139 = EDGE_CURVE ( 'NONE', #12686, #303, #16270, .T. ) ;
#3140 = CARTESIAN_POINT ( 'NONE',  ( 2.789999999999999147, 20.62201879784912606, 12.52067188844359080 ) ) ;
#3141 = LINE ( 'NONE', #18160, #2641 ) ;
#3142 = CIRCLE ( 'NONE', #16246, 3.000000000000000000 ) ;
#3143 = ORIENTED_EDGE ( 'NONE', *, *, #13340, .F. ) ;
#3144 = CARTESIAN_POINT ( 'NONE',  ( 1.749999999999998002, 12.52377138324259143, -25.12109765559640451 ) ) ;
#3145 = CARTESIAN_POINT ( 'NONE',  ( 4.233219804643871598, -2.444050593750019651, -11.46874999795161543 ) ) ;
#3146 = ORIENTED_EDGE ( 'NONE', *, *, #18220, .F. ) ;
#3147 = CARTESIAN_POINT ( 'NONE',  ( 4.942249507334556924, 0.2590123213420971182, -12.96874999795161543 ) ) ;
#3148 = VERTEX_POINT ( 'NONE', #300 ) ;
#3149 = SHAPE_DEFINITION_REPRESENTATION ( #16425, #451 ) ;
#3150 = CARTESIAN_POINT ( 'NONE',  ( 2.604434283110813819, 12.84444904262057818, -22.53097606932971075 ) ) ;
#3151 = CARTESIAN_POINT ( 'NONE',  ( 2.849999999999954348, -4.936344801571327601, -7.312499995903225525 ) ) ;
#3152 = VERTEX_POINT ( 'NONE', #9513 ) ;
#3153 = VERTEX_POINT ( 'NONE', #15609 ) ;
#3154 = CARTESIAN_POINT ( 'NONE',  ( 0.07181523211953061425, 10.24584646439538993, 23.19431517146936983 ) ) ;
#3155 = DIRECTION ( 'NONE',  ( 0.000000000000000000, 0.000000000000000000, 1.000000000000000000 ) ) ;
#3156 = EDGE_CURVE ( 'NONE', #2645, #13293, #6378, .T. ) ;
#3157 = ORIENTED_EDGE ( 'NONE', *, *, #14706, .F. ) ;
#3158 = VECTOR ( 'NONE', #11550, 1000.000000000000000 ) ;
#3159 = CARTESIAN_POINT ( 'NONE',  ( -1.310841663519413114, 0.000000000000000000, 4.000000000000000000 ) ) ;
#3160 = ORIENTED_EDGE ( 'NONE', *, *, #8723, .F. ) ;
#3161 = AXIS2_PLACEMENT_3D ( 'NONE', #14865, #12065, #10564 ) ;
#3162 = DIRECTION ( 'NONE',  ( 0.000000000000000000, -1.000000000000000000, 0.000000000000000000 ) ) ;
#3163 = FACE_OUTER_BOUND ( 'NONE', #3334, .T. ) ;
#3164 = EDGE_CURVE ( 'NONE', #9330, #7633, #6678, .T. ) ;
#3165 = DIRECTION ( 'NONE',  ( -1.000000000000000000, 0.000000000000000000, 0.000000000000000000 ) ) ;
#3166 = AXIS2_PLACEMENT_3D ( 'NONE', #14478, #3856, #17668 ) ;
#3167 = ORIENTED_EDGE ( 'NONE', *, *, #18231, .T. ) ;
#3168 = ORIENTED_EDGE ( 'NONE', *, *, #14281, .T. ) ;
#3169 = CARTESIAN_POINT ( 'NONE',  ( 1.749999999999998002, 0.000000000000000000, 0.000000000000000000 ) ) ;
#3170 =( NAMED_UNIT ( * ) PLANE_ANGLE_UNIT ( ) SI_UNIT ( $, .RADIAN. ) );
#3171 = DIRECTION ( 'NONE',  ( -1.000000000000000000, -0.000000000000000000, 0.000000000000000000 ) ) ;
#3172 = ORIENTED_EDGE ( 'NONE', *, *, #11273, .F. ) ;
#3173 = EDGE_LOOP ( 'NONE', ( #1745, #9621 ) ) ;
#3174 = CYLINDRICAL_SURFACE ( 'NONE', #14334, 8.000000000000000000 ) ;
#3175 = CYLINDRICAL_SURFACE ( 'NONE', #17801, 13.19999999999999929 ) ;
#3176 = CARTESIAN_POINT ( 'NONE',  ( -5.700000000000000178, -2.180340287075187351E-16, -12.66727757604271076 ) ) ;
#3177 = ADVANCED_FACE ( 'NONE', ( #7991, #6478 ), #12612, .T. ) ;
#3178 = CARTESIAN_POINT ( 'NONE',  ( 5.476417968967387750, 17.43449690031536292, -35.00000000000000000 ) ) ;
#3179 = CARTESIAN_POINT ( 'NONE',  ( 0.9027913098498566713, 5.699999999999999289, -11.50000000000000355 ) ) ;
#3180 = VERTEX_POINT ( 'NONE', #1995 ) ;
#3181 = CARTESIAN_POINT ( 'NONE',  ( -15.87499999999998579, -1.734723475976807094E-15, -6.527800000000000047 ) ) ;
#3182 = DIRECTION ( 'NONE',  ( 0.000000000000000000, 0.000000000000000000, 1.000000000000000000 ) ) ;
#3183 = ORIENTED_EDGE ( 'NONE', *, *, #4858, .F. ) ;
#3184 = DIRECTION ( 'NONE',  ( 1.000000000000000000, 0.000000000000000000, 0.000000000000000000 ) ) ;
#3185 = CARTESIAN_POINT ( 'NONE',  ( 7.937500000000000000, 0.000000000000000000, 0.000000000000000000 ) ) ;
#3186 = CIRCLE ( 'NONE', #14381, 1.000000000000000000 ) ;
#3187 = CIRCLE ( 'NONE', #13107, 2.524999999999995914 ) ;
#3188 = FACE_OUTER_BOUND ( 'NONE', #2681, .T. ) ;
#3189 = CARTESIAN_POINT ( 'NONE',  ( 2.783069004973550253, -23.92277630352791107, -5.408431875071696204 ) ) ;
#3190 = ORIENTED_EDGE ( 'NONE', *, *, #18445, .T. ) ;
#3191 = CARTESIAN_POINT ( 'NONE',  ( 10.50000000000000711, 5.699999999999999289, -0.9027913098498572264 ) ) ;
#3192 = CARTESIAN_POINT ( 'NONE',  ( 8.671566133830875600, 15.77352024078954784, -35.00000000000000000 ) ) ;
#3193 = FILL_AREA_STYLE_COLOUR ( '', #9941 ) ;
#3194 = VERTEX_POINT ( 'NONE', #14795 ) ;
#3195 = CARTESIAN_POINT ( 'NONE',  ( 0.000000000000000000, 0.000000000000000000, 0.000000000000000000 ) ) ;
#3196 = CARTESIAN_POINT ( 'NONE',  ( -16.11901729331276911, 5.562305898749051458, 32.00000000000000000 ) ) ;
#3197 = CARTESIAN_POINT ( 'NONE',  ( 1.394999999999998685, 25.12109765559671004, -12.52377138324198214 ) ) ;
#3198 = EDGE_CURVE ( 'NONE', #13000, #17134, #3888, .T. ) ;
#3199 = ORIENTED_EDGE ( 'NONE', *, *, #19720, .T. ) ;
#3200 = ADVANCED_FACE ( 'NONE', ( #10197, #15999 ), #13096, .F. ) ;
#3201 = CYLINDRICAL_SURFACE ( 'NONE', #13164, 4.762500000000000178 ) ;
#3202 = AXIS2_PLACEMENT_3D ( 'NONE', #4187, #14895, #8689 ) ;
#3203 = CARTESIAN_POINT ( 'NONE',  ( -4.888101187500000222, 0.7741991708318887166, -7.343749997951615427 ) ) ;
#3204 = TOROIDAL_SURFACE ( 'NONE', #13424, -21.04737509655562988, 30.00000000000000355 ) ;
#3205 = ORIENTED_EDGE ( 'NONE', *, *, #12349, .T. ) ;
#3206 = CARTESIAN_POINT ( 'NONE',  ( 13.96874999795161365, -3.499494075959791672, -3.499494075959840078 ) ) ;
#3207 = DIRECTION ( 'NONE',  ( 0.000000000000000000, 0.000000000000000000, 1.000000000000000000 ) ) ;
#3208 = VERTEX_POINT ( 'NONE', #7164 ) ;
#3209 = ADVANCED_FACE ( 'NONE', ( #8501 ), #2290, .F. ) ;
#3210 = CARTESIAN_POINT ( 'NONE',  ( 3.954556930911861112, 2.873153789725825913, -14.46874999795161720 ) ) ;
#3211 = CARTESIAN_POINT ( 'NONE',  ( 2.999999999999998224, 3.950217066951266176, -3.681818181818181213 ) ) ;
#3212 = EDGE_CURVE ( 'NONE', #12385, #15108, #3944, .T. ) ;
#3213 = ORIENTED_EDGE ( 'NONE', *, *, #9370, .T. ) ;
#3214 = CIRCLE ( 'NONE', #13439, 4.200000000000000178 ) ;
#3215 = FACE_OUTER_BOUND ( 'NONE', #9225, .T. ) ;
#3217 = ADVANCED_FACE ( 'NONE', ( #13003 ), #801, .T. ) ;
#3216 = EDGE_CURVE ( 'NONE', #17337, #8711, #17047, .T. ) ;
#3218 = AXIS2_PLACEMENT_3D ( 'NONE', #6429, #14356, #9562 ) ;
#3219 = FACE_OUTER_BOUND ( 'NONE', #9733, .T. ) ;
#3220 = ORIENTED_EDGE ( 'NONE', *, *, #14235, .F. ) ;
#3221 = CYLINDRICAL_SURFACE ( 'NONE', #4163, 7.500000000000000000 ) ;
#3222 = VERTEX_POINT ( 'NONE', #10297 ) ;
#3223 = CARTESIAN_POINT ( 'NONE',  ( 2.262072769566604524, -24.43806413951684320, 11.57956866523208461 ) ) ;
#3224 = ORIENTED_EDGE ( 'NONE', *, *, #774, .T. ) ;
#3225 = CARTESIAN_POINT ( 'NONE',  ( 2.299999999999998934, 0.000000000000000000, 0.000000000000000000 ) ) ;
#3226 = CARTESIAN_POINT ( 'NONE',  ( -4.233219804643904460, -2.444050593749961031, -11.84374999795161365 ) ) ;
#3227 = CARTESIAN_POINT ( 'NONE',  ( -2.000000000000001776, 1.012170579495290078E-15, 8.265000000000021885 ) ) ;
#3228 = CARTESIAN_POINT ( 'NONE',  ( 12.99999999999999467, 0.3952618871915727916, 4.872094134945738730 ) ) ;
#3229 = ORIENTED_EDGE ( 'NONE', *, *, #4667, .T. ) ;
#3230 = PLANE ( 'NONE',  #9037 ) ;
#3231 = CIRCLE ( 'NONE', #17301, 1.000000000000004441 ) ;
#3232 = DIRECTION ( 'NONE',  ( 0.000000000000000000, 0.000000000000000000, 1.000000000000000000 ) ) ;
#3233 = VECTOR ( 'NONE', #10284, 1000.000000000000000 ) ;
#3234 = EDGE_LOOP ( 'NONE', ( #15468, #11160, #10435, #3496, #2654, #13520 ) ) ;
#3235 = CARTESIAN_POINT ( 'NONE',  ( 0.7592463834391194322, -24.80264696524891477, 12.05220173035428921 ) ) ;
#3236 = CARTESIAN_POINT ( 'NONE',  ( 2.783025228907520798, -22.53337530003396338, -9.686319561461189664 ) ) ;
#3237 = VERTEX_POINT ( 'NONE', #6874 ) ;
#3238 = CARTESIAN_POINT ( 'NONE',  ( 2.257825459230522913, 26.58873630738059290, -4.993157874727537582 ) ) ;
#3239 = CYLINDRICAL_SURFACE ( 'NONE', #13599, 4.000000000000000000 ) ;
#3240 = EDGE_LOOP ( 'NONE', ( #6363, #18871, #3205, #14448 ) ) ;
#3241 = CARTESIAN_POINT ( 'NONE',  ( -2.000000000000000888, 7.500000000000000000, 0.000000000000000000 ) ) ;
#3242 = VECTOR ( 'NONE', #3510, 1000.000000000000000 ) ;
#3243 = ORIENTED_EDGE ( 'NONE', *, *, #16183, .T. ) ;
#3244 = APPLICATION_PROTOCOL_DEFINITION ( 'draft international standard', 'automotive_design', 1998, #13915 ) ;
#3245 = AXIS2_PLACEMENT_3D ( 'NONE', #18906, #12812, #13102 ) ;
#3246 = FACE_OUTER_BOUND ( 'NONE', #3907, .T. ) ;
#3247 = CARTESIAN_POINT ( 'NONE',  ( 6.843749997951615427, 4.233219804643887585, -2.444050593749990341 ) ) ;
#3248 = AXIS2_PLACEMENT_3D ( 'NONE', #1415, #19415, #8816 ) ;
#3249 = VERTEX_POINT ( 'NONE', #5387 ) ;
#3250 = ORIENTED_EDGE ( 'NONE', *, *, #11657, .F. ) ;
#3251 = DIRECTION ( 'NONE',  ( -1.000000000000000000, 1.224646799147353207E-16, 0.000000000000000000 ) ) ;
#3252 = B_SPLINE_CURVE_WITH_KNOTS ( 'NONE', 3,
 ( #10799, #12602, #5081, #11194 ),
 .UNSPECIFIED., .F., .F.,
 ( 4, 4 ),
 ( 0.005258120783916792398, 0.005948386350302926374 ),
 .UNSPECIFIED. ) ;
#3253 = CARTESIAN_POINT ( 'NONE',  ( 4.942249507334556924, 0.2590123213420975623, -13.34374999795161365 ) ) ;
#3254 = ORIENTED_EDGE ( 'NONE', *, *, #10304, .F. ) ;
#3255 = DIRECTION ( 'NONE',  ( 0.000000000000000000, 0.000000000000000000, -1.000000000000000000 ) ) ;
#3256 = VECTOR ( 'NONE', #6278, 1000.000000000000000 ) ;
#3257 = EDGE_LOOP ( 'NONE', ( #4050, #7202 ) ) ;
#3258 = AXIS2_PLACEMENT_3D ( 'NONE', #17779, #5858, #19174 ) ;
#3259 = AXIS2_PLACEMENT_3D ( 'NONE', #15095, #4779, #13589 ) ;
#3260 = CARTESIAN_POINT ( 'NONE',  ( 1.185096637661176677, -5.575441324182703440, -7.000000000000005329 ) ) ;
#3261 = EDGE_CURVE ( 'NONE', #17434, #4324, #5675, .T. ) ;
#3262 = AXIS2_PLACEMENT_3D ( 'NONE', #10978, #7770, #6352 ) ;
#3263 = FACE_OUTER_BOUND ( 'NONE', #224, .T. ) ;
#3264 = FACE_BOUND ( 'NONE', #17721, .T. ) ;
#3265 = ORIENTED_EDGE ( 'NONE', *, *, #4373, .F. ) ;
#3266 = DIRECTION ( 'NONE',  ( 0.000000000000000000, 0.000000000000000000, 1.000000000000000000 ) ) ;
#3267 = SHAPE_REPRESENTATION_RELATIONSHIP ( 'NONE' , 'NONE' ,  #2475, #7075 ) ;
#3268 = VERTEX_POINT ( 'NONE', #8687 ) ;
#3269 = ORIENTED_EDGE ( 'NONE', *, *, #17032, .T. ) ;
#3270 = DIRECTION ( 'NONE',  ( 1.000000000000000000, 0.000000000000000000, 0.000000000000000000 ) ) ;
#3271 = ADVANCED_BREP_SHAPE_REPRESENTATION ( '', ( #9200, #16724 ), #3651 ) ;
#3272 = CARTESIAN_POINT ( 'NONE',  ( -5.574407415329146964, 1.493657965219562067, -14.81249999590322552 ) ) ;
#3273 = VECTOR ( 'NONE', #9878, 1000.000000000000000 ) ;
#3274 = DIRECTION ( 'NONE',  ( 0.000000000000000000, 0.000000000000000000, 1.000000000000000000 ) ) ;
#3275 = AXIS2_PLACEMENT_3D ( 'NONE', #15712, #12907, #6784 ) ;
#3276 = CARTESIAN_POINT ( 'NONE',  ( 9.671566133830877376, 15.77352024078954784, 32.00000000000000000 ) ) ;
#3277 = AXIS2_PLACEMENT_3D ( 'NONE', #3733, #6820, #12943 ) ;
#3278 = CARTESIAN_POINT ( 'NONE',  ( 3.954556930911861112, 2.873153789725825913, -14.46874999795161720 ) ) ;
#3279 = VERTEX_POINT ( 'NONE', #10008 ) ;
#3280 = DIRECTION ( 'NONE',  ( 1.000000000000000000, 0.000000000000000000, 0.000000000000000000 ) ) ;
#3281 = VECTOR ( 'NONE', #9063, 1000.000000000000000 ) ;
#3282 = EDGE_CURVE ( 'NONE', #2239, #12054, #16394, .T. ) ;
#3283 = CARTESIAN_POINT ( 'NONE',  ( 8.343749997951613651, -2.246813503491864150, 4.409619785863891472 ) ) ;
#3284 = ORIENTED_EDGE ( 'NONE', *, *, #9449, .F. ) ;
#3285 = CARTESIAN_POINT ( 'NONE',  ( 9.000000000000000000, 1.102182119232617714E-15, -33.00000000000000000 ) ) ;
#3286 = CARTESIAN_POINT ( 'NONE',  ( 7.937500000000001776, 0.7748640365313755884, -6.324512672832110842E-17 ) ) ;
#3287 =( GEOMETRIC_REPRESENTATION_CONTEXT ( 3 ) GLOBAL_UNCERTAINTY_ASSIGNED_CONTEXT ( ( #11595 ) ) GLOBAL_UNIT_ASSIGNED_CONTEXT ( ( #4650, #7743, #12360 ) ) REPRESENTATION_CONTEXT ( 'NONE', 'WORKASPACE' ) );
#3288 = B_SPLINE_CURVE_WITH_KNOTS ( 'NONE', 3,
 ( #17524, #13024, #11424, #1003, #10219, #19304 ),
 .UNSPECIFIED., .F., .F.,
 ( 4, 2, 4 ),
 ( 4.462636808935014747E-07, 0.001879885123572234236, 0.003759323983463574645 ),
 .UNSPECIFIED. ) ;
#3289 = EDGE_CURVE ( 'NONE', #17537, #15386, #9698, .T. ) ;
#3290 = CARTESIAN_POINT ( 'NONE',  ( 8.000000000000000000, 0.000000000000000000, 0.000000000000000000 ) ) ;
#3291 = CARTESIAN_POINT ( 'NONE',  ( 3.476417968967386418, 17.43449690031536292, -35.00000000000000000 ) ) ;
#3292 = CARTESIAN_POINT ( 'NONE',  ( 2.789999999999999147, 24.63872515616082737, 2.336989772644355146 ) ) ;
#3293 = ORIENTED_EDGE ( 'NONE', *, *, #12127, .F. ) ;
#3294 = AXIS2_PLACEMENT_3D ( 'NONE', #3737, #8138, #15948 ) ;
#3295 = CARTESIAN_POINT ( 'NONE',  ( 8.000000000000000000, 0.000000000000000000, 0.000000000000000000 ) ) ;
#3296 = DIRECTION ( 'NONE',  ( -0.000000000000000000, -0.000000000000000000, 1.000000000000000000 ) ) ;
#3297 = B_SPLINE_CURVE_WITH_KNOTS ( 'NONE', 1,
 ( #1392, #18294 ),
 .UNSPECIFIED., .F., .F.,
 ( 2, 2 ),
 ( 0.000000000000000000, 1.000000000000000000 ),
 .UNSPECIFIED. ) ;
#3298 = AXIS2_PLACEMENT_3D ( 'NONE', #17503, #13196, #2477 ) ;
#3299 = LINE ( 'NONE', #13706, #7681 ) ;
#3300 = ORIENTED_EDGE ( 'NONE', *, *, #4939, .T. ) ;
#3301 = CARTESIAN_POINT ( 'NONE',  ( -36.00000000000000000, -2.000000000000000888, -2.000000000000000000 ) ) ;
#3302 = CARTESIAN_POINT ( 'NONE',  ( 8.968749997951611874, 4.780397808154257078, 1.280903732194454303 ) ) ;
#3303 = CARTESIAN_POINT ( 'NONE',  ( 0.0001048300153468720319, 20.67846228565678146, -12.51925356660738053 ) ) ;
#3304 = ORIENTED_EDGE ( 'NONE', *, *, #3354, .F. ) ;
#3305 = CYLINDRICAL_SURFACE ( 'NONE', #13803, 2.524999999999997691 ) ;
#3306 = STYLED_ITEM ( 'NONE', ( #17790 ), #17347 ) ;
#3307 = DIRECTION ( 'NONE',  ( -0.000000000000000000, -0.000000000000000000, 1.000000000000000000 ) ) ;
#3308 = ORIENTED_EDGE ( 'NONE', *, *, #1838, .T. ) ;
#3309 = CARTESIAN_POINT ( 'NONE',  ( 7.000000000000005329, -3.814044456245443193, -4.235925505221191933 ) ) ;
#3310 = EDGE_CURVE ( 'NONE', #6550, #4244, #760, .T. ) ;
#3311 = CARTESIAN_POINT ( 'NONE',  ( 2.790000000000076419, -2.133839912090968127, 24.22524813288760726 ) ) ;
#3312 = ORIENTED_EDGE ( 'NONE', *, *, #8331, .T. ) ;
#3313 = CIRCLE ( 'NONE', #4913, 28.06981291497571362 ) ;
#3314 = ITEM_DEFINED_TRANSFORMATION ( 'NONE', 'NONE', #2203,  #16724 ) ;
#3315 = ADVANCED_FACE ( 'NONE', ( #11593 ), #13288, .T. ) ;
#3316 = DIRECTION ( 'NONE',  ( -0.000000000000000000, -0.000000000000000000, 1.000000000000000000 ) ) ;
#3317 = FACE_OUTER_BOUND ( 'NONE', #3696, .T. ) ;
#3318 = ADVANCED_FACE ( 'NONE', ( #17696 ), #3991, .F. ) ;
#3319 = ORIENTED_EDGE ( 'NONE', *, *, #11844, .T. ) ;
#3320 = MECHANICAL_DESIGN_GEOMETRIC_PRESENTATION_REPRESENTATION (  '', ( #8761 ), #10990 ) ;
#3321 = CARTESIAN_POINT ( 'NONE',  ( 2.765633920072235963, -24.63872515616080960, -2.336989772644527008 ) ) ;
#3322 = DIRECTION ( 'NONE',  ( 1.000000000000000000, 6.419766481290786633E-33, -0.000000000000000000 ) ) ;
#3323 = ORIENTED_EDGE ( 'NONE', *, *, #3554, .F. ) ;
#3324 = DIRECTION ( 'NONE',  ( -1.000000000000000000, 0.000000000000000000, -0.000000000000000000 ) ) ;
#3325 = EDGE_LOOP ( 'NONE', ( #13310, #3374, #3961, #1678 ) ) ;
#3326 = DIRECTION ( 'NONE',  ( -0.000000000000000000, -0.000000000000000000, 1.000000000000000000 ) ) ;
#3327 = ORIENTED_EDGE ( 'NONE', *, *, #5451, .F. ) ;
#3328 = CARTESIAN_POINT ( 'NONE',  ( 2.031033465052725084, -4.828387785248216879, 27.14933624560906367 ) ) ;
#3329 = CIRCLE ( 'NONE', #3007, 1.000000000000000888 ) ;
#3330 = CARTESIAN_POINT ( 'NONE',  ( 1.773574444220693103, -4.620319390059841602, -7.343749997951615427 ) ) ;
#3331 = EDGE_CURVE ( 'NONE', #15782, #8799, #14497, .T. ) ;
#3332 = B_SPLINE_CURVE_WITH_KNOTS ( 'NONE', 3,
 ( #9490, #3377, #17086, #12483 ),
 .UNSPECIFIED., .F., .F.,
 ( 4, 4 ),
 ( 2.324263106244698315E-07, 0.0006888201370294716810 ),
 .UNSPECIFIED. ) ;
#3333 = CARTESIAN_POINT ( 'NONE',  ( 0.5109457054261454800, -4.861323657744410554, -14.46874999795161720 ) ) ;
#3334 = EDGE_LOOP ( 'NONE', ( #8820, #5201, #15772, #15557, #2606, #2299 ) ) ;
#3335 = DIRECTION ( 'NONE',  ( -1.000000000000000000, 0.000000000000000000, 0.000000000000000000 ) ) ;
#3336 = AXIS2_PLACEMENT_3D ( 'NONE', #8245, #5434, #6724 ) ;
#3337 = EDGE_CURVE ( 'NONE', #14452, #12361, #19589, .T. ) ;
#3338 = CARTESIAN_POINT ( 'NONE',  ( 2.789999999999999147, 18.28042085475278355, 15.74360496233388140 ) ) ;
#3339 = EDGE_CURVE ( 'NONE', #11363, #17434, #14799, .T. ) ;
#3340 = VERTEX_POINT ( 'NONE', #9914 ) ;
#3341 = CIRCLE ( 'NONE', #15794, 28.06981291497571362 ) ;
#3342 = CARTESIAN_POINT ( 'NONE',  ( 2.765633920072235519, 24.15498966839970052, -5.391175441198366336 ) ) ;
#3343 = CARTESIAN_POINT ( 'NONE',  ( -3.846120219227966430, -3.114526743279228072, -10.96874999795161720 ) ) ;
#3344 = VERTEX_POINT ( 'NONE', #11690 ) ;
#3345 = CARTESIAN_POINT ( 'NONE',  ( 7.500000000000005329, -5.763142191869158992, 0.3020334839682081163 ) ) ;
#3346 = CARTESIAN_POINT ( 'NONE',  ( 0.000000000000000000, 9.324097380959415204, 22.25075486061743391 ) ) ;
#3347 = ORIENTED_EDGE ( 'NONE', *, *, #7702, .F. ) ;
#3348 = CARTESIAN_POINT ( 'NONE',  ( 0.000000000000000000, -20.62201879784905501, -12.52067188844372936 ) ) ;
#3349 = ORIENTED_EDGE ( 'NONE', *, *, #14817, .T. ) ;
#3350 = APPLICATION_PROTOCOL_DEFINITION ( 'draft international standard', 'automotive_design', 1998, #5712 ) ;
#3351 = FACE_OUTER_BOUND ( 'NONE', #10262, .T. ) ;
#3352 = DIRECTION ( 'NONE',  ( 1.000000000000000000, -0.000000000000000000, -0.000000000000000000 ) ) ;
#3353 = EDGE_CURVE ( 'NONE', #13895, #11363, #12291, .T. ) ;
#3354 = EDGE_CURVE ( 'NONE', #11311, #8927, #8088, .T. ) ;
#3355 = EDGE_LOOP ( 'NONE', ( #8266, #15339 ) ) ;
#3356 = ORIENTED_EDGE ( 'NONE', *, *, #18779, .T. ) ;
#3357 = CARTESIAN_POINT ( 'NONE',  ( 0.02436607992776498519, 9.836394144775706394, 22.71065055754456097 ) ) ;
#3358 = DIRECTION ( 'NONE',  ( -0.000000000000000000, 0.000000000000000000, 1.000000000000000000 ) ) ;
#3359 = EDGE_LOOP ( 'NONE', ( #17713, #7279 ) ) ;
#3360 = EDGE_CURVE ( 'NONE', #10459, #5854, #7762, .T. ) ;
#3361 = ADVANCED_FACE ( 'NONE', ( #18386 ), #7467, .T. ) ;
#3362 = DIRECTION ( 'NONE',  ( 0.000000000000000000, -0.3090169943749406234, -0.9510565162951558627 ) ) ;
#3363 = VECTOR ( 'NONE', #11699, 1000.000000000000000 ) ;
#3364 = ORIENTED_EDGE ( 'NONE', *, *, #4183, .T. ) ;
#3365 = CIRCLE ( 'NONE', #15147, 9.000000000000000000 ) ;
#3366 = DIRECTION ( 'NONE',  ( 1.000000000000000000, 0.000000000000000000, 0.000000000000000000 ) ) ;
#3367 = CYLINDRICAL_SURFACE ( 'NONE', #92, 1.000000000000004441 ) ;
#3368 = FACE_BOUND ( 'NONE', #13849, .T. ) ;
#3369 = ORIENTED_EDGE ( 'NONE', *, *, #7061, .F. ) ;
#3370 = LINE ( 'NONE', #9482, #18442 ) ;
#3371 = FILL_AREA_STYLE_COLOUR ( '', #3963 ) ;
#3372 = ADVANCED_FACE ( 'NONE', ( #2874 ), #3175, .T. ) ;
#3373 = ORIENTED_EDGE ( 'NONE', *, *, #19677, .F. ) ;
#3374 = ORIENTED_EDGE ( 'NONE', *, *, #17291, .T. ) ;
#3375 = CARTESIAN_POINT ( 'NONE',  ( 1.749999999999998002, 4.633866840649310426, -27.68468304288254345 ) ) ;
#3376 = AXIS2_PLACEMENT_3D ( 'NONE', #10742, #18729, #12245 ) ;
#3377 = CARTESIAN_POINT ( 'NONE',  ( 0.006974693931643255289, 16.17543236987988919, 18.43727551351037519 ) ) ;
#3378 = CARTESIAN_POINT ( 'NONE',  ( 17.68117051311639898, -3.372863662543048591, -32.00000000000000000 ) ) ;
#3379 = CIRCLE ( 'NONE', #14252, 4.400000000000000355 ) ;
#3380 = DIRECTION ( 'NONE',  ( 1.000000000000000000, -0.000000000000000000, -0.000000000000000000 ) ) ;
#3381 = CARTESIAN_POINT ( 'NONE',  ( -1.493657965219446382, 5.574407415329178939, -14.81249999590322552 ) ) ;
#3382 = ADVANCED_FACE ( 'NONE', ( #4581, #13688, #17999, #6070, #4286, #1386, #3075, #1285, #1681, #11887, #5769, #8889, #9189, #4680, #15294, #8987, #14990, #1579, #78, #10785, #7360, #4383, #13586, #16593, #19686, #16694, #15091 ), #12092, .F. ) ;
#3383 = ORIENTED_EDGE ( 'NONE', *, *, #4312, .T. ) ;
#3384 = LINE ( 'NONE', #16806, #1349 ) ;
#3385 = CARTESIAN_POINT ( 'NONE',  ( 11.34374999795161543, -4.888101187500005551, 0.7741991708318548548 ) ) ;
#3386 = EDGE_LOOP ( 'NONE', ( #12658, #18758, #13143, #5921, #14658 ) ) ;
#3387 = DIRECTION ( 'NONE',  ( 0.000000000000000000, 0.000000000000000000, 1.000000000000000000 ) ) ;
#3388 = DIRECTION ( 'NONE',  ( 0.000000000000000000, 0.000000000000000000, -1.000000000000000000 ) ) ;
#3389 = VECTOR ( 'NONE', #5406, 1000.000000000000000 ) ;
#3390 = ADVANCED_FACE ( 'NONE', ( #16497 ), #15389, .F. ) ;
#3391 = VECTOR ( 'NONE', #12519, 1000.000000000000000 ) ;
#3392 = CARTESIAN_POINT ( 'NONE',  ( -5.574407415329178939, -1.493657965219446160, -9.812499995903225525 ) ) ;
#3393 = CARTESIAN_POINT ( 'NONE',  ( 2.789999999999999147, 24.34211360614310848, -7.909232158574561744 ) ) ;
#3394 = CARTESIAN_POINT ( 'NONE',  ( 1.761396867937162769, -5.421022142882388373, -10.00000000000000533 ) ) ;
#3395 = VERTEX_POINT ( 'NONE', #2976 ) ;
#3396 = FACE_OUTER_BOUND ( 'NONE', #12351, .T. ) ;
#3397 = DIRECTION ( 'NONE',  ( -1.000000000000000000, 0.000000000000000000, -0.000000000000000000 ) ) ;
#3398 = DIRECTION ( 'NONE',  ( 0.000000000000000000, 0.000000000000000000, 1.000000000000000000 ) ) ;
#3399 = ORIENTED_EDGE ( 'NONE', *, *, #19726, .T. ) ;
#3400 = CARTESIAN_POINT ( 'NONE',  ( -1.799999999999999600, 0.000000000000000000, 0.000000000000000000 ) ) ;
#3401 = CARTESIAN_POINT ( 'NONE',  ( -1.255998204157475318, -17.85806462366060288, 32.00000000000000000 ) ) ;
#3402 = CARTESIAN_POINT ( 'NONE',  ( 5.387740456496221242, -2.068159791354220900, -10.50000000000000533 ) ) ;
#3403 = DIRECTION ( 'NONE',  ( 1.000000000000000000, 0.000000000000000000, 0.000000000000000000 ) ) ;
#3404 = CARTESIAN_POINT ( 'NONE',  ( -2.647025296874989664, 4.584782303107598267, -6.234374998975811266 ) ) ;
#3405 = VERTEX_POINT ( 'NONE', #13481 ) ;
#3406 = CARTESIAN_POINT ( 'NONE',  ( 16.68117051311640253, -3.372863662543048591, 32.00000000000000000 ) ) ;
#3407 = AXIS2_PLACEMENT_3D ( 'NONE', #2380, #14601, #6968 ) ;
#3408 = LINE ( 'NONE', #14309, #12409 ) ;
#3409 = EDGE_CURVE ( 'NONE', #758, #3208, #5875, .T. ) ;
#3410 = CIRCLE ( 'NONE', #11717, 8.800000000000023803 ) ;
#3411 = ORIENTED_EDGE ( 'NONE', *, *, #6990, .T. ) ;
#3412 = DIRECTION ( 'NONE',  ( -1.000000000000000000, 0.000000000000000000, -0.000000000000000000 ) ) ;
#3413 = CYLINDRICAL_SURFACE ( 'NONE', #1788, 1.000000000000004441 ) ;
#3414 = ORIENTED_EDGE ( 'NONE', *, *, #19473, .F. ) ;
#3415 = LINE ( 'NONE', #8210, #2924 ) ;
#3416 = CARTESIAN_POINT ( 'NONE',  ( -19.00000000000000355, -4.898587196589412829E-16, 0.000000000000000000 ) ) ;
#3417 = ORIENTED_EDGE ( 'NONE', *, *, #2322, .T. ) ;
#3418 = AXIS2_PLACEMENT_3D ( 'NONE', #1675, #267, #7564 ) ;
#3419 = LINE ( 'NONE', #4721, #18086 ) ;
#3420 = CARTESIAN_POINT ( 'NONE',  ( 16.28688694438835327, -7.664027248171309203, 32.00000000000000000 ) ) ;
#3421 = EDGE_LOOP ( 'NONE', ( #16276, #13714, #628, #16669 ) ) ;
#3422 = EDGE_CURVE ( 'NONE', #18407, #2052, #18195, .T. ) ;
#3423 = DIRECTION ( 'NONE',  ( 0.000000000000000000, -0.7806247497997995666, 0.6250000000000001110 ) ) ;
#3424 = EDGE_LOOP ( 'NONE', ( #15892, #7889, #1986, #7366 ) ) ;
#3425 = EDGE_CURVE ( 'NONE', #9243, #2241, #7233, .T. ) ;
#3426 = CARTESIAN_POINT ( 'NONE',  ( 1.749999999999998002, -25.12109765559663188, 12.52377138324213668 ) ) ;
#3427 = ORIENTED_EDGE ( 'NONE', *, *, #1563, .F. ) ;
#3428 = CARTESIAN_POINT ( 'NONE',  ( -17.96448111170888851, 1.130229351527647585, -32.00000000000000000 ) ) ;
#3429 = DIRECTION ( 'NONE',  ( -0.5877852522924721379, 0.8090169943749482284, 0.000000000000000000 ) ) ;
#3430 = CARTESIAN_POINT ( 'NONE',  ( 16.28688694438835327, -7.664027248171309203, -35.00000000000000000 ) ) ;
#3431 = FACE_OUTER_BOUND ( 'NONE', #14729, .T. ) ;
#3432 = EDGE_CURVE ( 'NONE', #7344, #11827, #1175, .T. ) ;
#3433 = ORIENTED_EDGE ( 'NONE', *, *, #11726, .F. ) ;
#3434 = CARTESIAN_POINT ( 'NONE',  ( 5.626241948324195441, -16.73597674598852691, 32.00000000000000000 ) ) ;
#3435 = DIRECTION ( 'NONE',  ( 0.000000000000000000, 0.8090169943749400128, 0.5877852522924831291 ) ) ;
#3436 = AXIS2_PLACEMENT_3D ( 'NONE', #11520, #2501, #5506 ) ;
#3437 = ORIENTED_EDGE ( 'NONE', *, *, #6981, .F. ) ;
#3438 = VECTOR ( 'NONE', #5443, 1000.000000000000000 ) ;
#3439 = DIRECTION ( 'NONE',  ( 6.419766481290786633E-33, -1.000000000000000000, 0.000000000000000000 ) ) ;
#3440 = DIRECTION ( 'NONE',  ( 0.000000000000000000, 1.000000000000000000, 0.000000000000000000 ) ) ;
#3441 = CARTESIAN_POINT ( 'NONE',  ( 1.039999999999997593, 0.000000000000000000, 0.000000000000000000 ) ) ;
#3442 = ORIENTED_EDGE ( 'NONE', *, *, #8852, .T. ) ;
#3443 = CARTESIAN_POINT ( 'NONE',  ( 0.000000000000000000, 0.000000000000000000, 0.000000000000000000 ) ) ;
#3444 = CARTESIAN_POINT ( 'NONE',  ( 8.343749997951611874, -2.695436003842674566, -4.150607464521828938 ) ) ;
#3445 = B_SPLINE_CURVE_WITH_KNOTS ( 'NONE', 3,
 ( #16789, #9275, #1671, #13775 ),
 .UNSPECIFIED., .F., .F.,
 ( 4, 4 ),
 ( 2.324263106244698315E-07, 0.0006888201370294677779 ),
 .UNSPECIFIED. ) ;
#3446 = ORIENTED_EDGE ( 'NONE', *, *, #1879, .T. ) ;
#3447 = FACE_BOUND ( 'NONE', #14696, .T. ) ;
#3448 = ORIENTED_EDGE ( 'NONE', *, *, #18107, .F. ) ;
#3449 = SHAPE_DEFINITION_REPRESENTATION ( #13226, #14878 ) ;
#3450 = CARTESIAN_POINT ( 'NONE',  ( -1.493657965219562511, -5.574407415329147852, -8.500000000000007105 ) ) ;
#3451 = VECTOR ( 'NONE', #7898, 1000.000000000000000 ) ;
#3452 = CARTESIAN_POINT ( 'NONE',  ( 10.96874999795161720, 3.114526743279255161, 3.846120219227944670 ) ) ;
#3453 = VERTEX_POINT ( 'NONE', #9388 ) ;
#3454 = ORIENTED_EDGE ( 'NONE', *, *, #6025, .F. ) ;
#3455 = CARTESIAN_POINT ( 'NONE',  ( 0.000000000000000000, 0.000000000000000000, 0.000000000000000000 ) ) ;
#3456 = LINE ( 'NONE', #8044, #10789 ) ;
#3457 = ORIENTED_EDGE ( 'NONE', *, *, #6080, .F. ) ;
#3458 = EDGE_CURVE ( 'NONE', #3222, #14330, #2152, .T. ) ;
#3459 = EDGE_CURVE ( 'NONE', #15555, #18641, #3332, .T. ) ;
#3460 = VECTOR ( 'NONE', #19558, 1000.000000000000000 ) ;
#3461 = ORIENTED_EDGE ( 'NONE', *, *, #13010, .F. ) ;
#3462 = AXIS2_PLACEMENT_3D ( 'NONE', #11892, #16699, #2677 ) ;
#3463 = ADVANCED_FACE ( 'NONE', ( #13887 ), #14595, .T. ) ;
#3464 = CARTESIAN_POINT ( 'NONE',  ( 2.068159791354145849, -5.387740456496247887, -6.500000000000005329 ) ) ;
#3465 = CARTESIAN_POINT ( 'NONE',  ( -2.000000000000001776, 0.000000000000000000, 0.000000000000000000 ) ) ;
#3466 = CARTESIAN_POINT ( 'NONE',  ( 0.000000000000000000, -15.04425356660744839, -18.18163861606288378 ) ) ;
#3467 = ORIENTED_EDGE ( 'NONE', *, *, #9342, .T. ) ;
#3468 = CARTESIAN_POINT ( 'NONE',  ( -16.68117051311640253, -3.372863662543042818, 35.00000000000000000 ) ) ;
#3469 = SURFACE_STYLE_USAGE ( .BOTH. , #14173 ) ;
#3470 = ADVANCED_FACE ( 'NONE', ( #9441 ), #18533, .T. ) ;
#3471 = CARTESIAN_POINT ( 'NONE',  ( -3.968750000000000000, 4.860316984116057109E-16, -0.5557897334539606549 ) ) ;
#3472 = ORIENTED_EDGE ( 'NONE', *, *, #6862, .T. ) ;
#3473 = ORIENTED_EDGE ( 'NONE', *, *, #1258, .T. ) ;
#3474 = CARTESIAN_POINT ( 'NONE',  ( -41.99999999999999289, -5.000000000000001776, -2.000000000000000000 ) ) ;
#3475 = VECTOR ( 'NONE', #5538, 1000.000000000000114 ) ;
#3476 = CARTESIAN_POINT ( 'NONE',  ( 1.749999999999998002, 0.000000000000000000, 0.000000000000000000 ) ) ;
#3477 = CARTESIAN_POINT ( 'NONE',  ( -4.233219804643852946, 2.444050593750049405, -11.84374999795161365 ) ) ;
#3478 = PRODUCT_DEFINITION_FORMATION_WITH_SPECIFIED_SOURCE ( 'ANY', '', #1243, .NOT_KNOWN. ) ;
#3479 = ORIENTED_EDGE ( 'NONE', *, *, #6249, .T. ) ;
#3480 = DIRECTION ( 'NONE',  ( 1.000000000000000000, 0.000000000000000000, 0.000000000000000000 ) ) ;
#3481 =( BOUNDED_CURVE ( )  B_SPLINE_CURVE ( 2, ( #10155, #8255, #18857, #16062, #5442, #4048, #2533, #564, #5248 ),
 .UNSPECIFIED., .F., .F. ) 
 B_SPLINE_CURVE_WITH_KNOTS ( ( 3, 2, 2, 2, 3 ),
 ( 0.000000000000000000, 0.04999999999999999584, 0.09999999999999999167, 0.1499999999999999944, 0.1666819079834116757 ),
 .UNSPECIFIED. ) 
 CURVE ( )  GEOMETRIC_REPRESENTATION_ITEM ( )  RATIONAL_B_SPLINE_CURVE ( ( 1.000000000000000000, 0.9876883405951377704, 1.000000000000000000, 0.9876883405951377704, 1.000000000000000000, 0.9876883405951377704, 1.000000000000000000, 0.9958923606136996787, 0.9945256517182512468 ) ) 
 REPRESENTATION_ITEM ( '' )  );
#3482 = CYLINDRICAL_SURFACE ( 'NONE', #10128, 7.174999999999998934 ) ;
#3483 =( REPRESENTATION_RELATIONSHIP ('NONE','NONE', #18211, #2588 ) REPRESENTATION_RELATIONSHIP_WITH_TRANSFORMATION ( #5436 )SHAPE_REPRESENTATION_RELATIONSHIP( ) );
#3484 = EDGE_LOOP ( 'NONE', ( #4196, #9221, #8840, #10800 ) ) ;
#3485 = CARTESIAN_POINT ( 'NONE',  ( 13.96874999795161365, 4.780397808154273065, -1.280903732194386802 ) ) ;
#3486 = EDGE_CURVE ( 'NONE', #608, #15823, #14130, .T. ) ;
#3487 = DIRECTION ( 'NONE',  ( 1.000000000000000000, 0.000000000000000000, 0.000000000000000000 ) ) ;
#3488 = VECTOR ( 'NONE', #12470, 1000.000000000000000 ) ;
#3489 = DIRECTION ( 'NONE',  ( 0.000000000000000000, 0.000000000000000000, 1.000000000000000000 ) ) ;
#3490 = FACE_OUTER_BOUND ( 'NONE', #5663, .T. ) ;
#3491 = CARTESIAN_POINT ( 'NONE',  ( 0.000000000000000000, -23.48180575137736170, 5.535312321042622052 ) ) ;
#3492 = EDGE_LOOP ( 'NONE', ( #1111, #2539, #14378, #7011, #7147, #2065 ) ) ;
#3493 = CARTESIAN_POINT ( 'NONE',  ( 1.960886852992497653, -24.44424927289185590, 12.96989951879399072 ) ) ;
#3494 = CARTESIAN_POINT ( 'NONE',  ( -2.000000000000001776, 0.000000000000000000, -8.073750000000021743 ) ) ;
#3495 = DIRECTION ( 'NONE',  ( 0.000000000000000000, 0.000000000000000000, 1.000000000000000000 ) ) ;
#3496 = ORIENTED_EDGE ( 'NONE', *, *, #2355, .F. ) ;
#3497 = DIRECTION ( 'NONE',  ( -1.000000000000000000, -0.000000000000000000, -0.000000000000000000 ) ) ;
#3498 = PLANE ( 'NONE',  #10025 ) ;
#3499 = CARTESIAN_POINT ( 'NONE',  ( 10.96874999795161720, 3.114526743279255161, 3.846120219227944670 ) ) ;
#3500 = DIRECTION ( 'NONE',  ( 1.000000000000000000, 0.000000000000000000, 0.000000000000000000 ) ) ;
#3501 = LINE ( 'NONE', #15710, #13378 ) ;
#3502 = ORIENTED_EDGE ( 'NONE', *, *, #18969, .F. ) ;
#3503 = DIRECTION ( 'NONE',  ( -1.000000000000000000, -0.000000000000000000, -0.000000000000000000 ) ) ;
#3504 = CARTESIAN_POINT ( 'NONE',  ( -2.000000000000001776, 0.000000000000000000, 0.000000000000000000 ) ) ;
#3505 = ORIENTED_EDGE ( 'NONE', *, *, #1827, .T. ) ;
#3506 = CARTESIAN_POINT ( 'NONE',  ( 12.96874999795161543, -4.409619785863891472, -2.246813503491864150 ) ) ;
#3507 = FACE_OUTER_BOUND ( 'NONE', #13416, .T. ) ;
#3508 = VECTOR ( 'NONE', #9064, 1000.000000000000000 ) ;
#3509 = EDGE_LOOP ( 'NONE', ( #2020, #10777, #464, #19765 ) ) ;
#3510 = DIRECTION ( 'NONE',  ( 0.000000000000000000, 0.000000000000000000, -1.000000000000000000 ) ) ;
#3511 = CARTESIAN_POINT ( 'NONE',  ( 12.31249999590322552, 5.700000000000001066, -3.490243377569957047E-16 ) ) ;
#3512 = ORIENTED_EDGE ( 'NONE', *, *, #11223, .T. ) ;
#3513 = CARTESIAN_POINT ( 'NONE',  ( 2.030753605846573162, -27.31305418910207905, -3.797885586973501759 ) ) ;
#3514 = LINE ( 'NONE', #12429, #18350 ) ;
#3515 = EDGE_CURVE ( 'NONE', #17485, #3138, #14918, .T. ) ;
#3516 = ORIENTED_EDGE ( 'NONE', *, *, #9638, .T. ) ;
#3517 = DIRECTION ( 'NONE',  ( 0.000000000000000000, 0.000000000000000000, 1.000000000000000000 ) ) ;
#3518 = VERTEX_POINT ( 'NONE', #6509 ) ;
#3519 = CARTESIAN_POINT ( 'NONE',  ( 2.790000000000000480, -22.37986894186679265, 9.514945144208653005 ) ) ;
#3520 = ORIENTED_EDGE ( 'NONE', *, *, #15902, .T. ) ;
#3521 = CIRCLE ( 'NONE', #16290, 0.2000000000000005107 ) ;
#3522 = VECTOR ( 'NONE', #18626, 1000.000000000000000 ) ;
#3523 = CARTESIAN_POINT ( 'NONE',  ( 2.604434325169354913, 2.851997810081644769, 25.77772010606606301 ) ) ;
#3524 = DIRECTION ( 'NONE',  ( -1.000000000000000000, -0.000000000000000000, -0.000000000000000000 ) ) ;
#3525 = DIRECTION ( 'NONE',  ( -0.000000000000000000, 0.6818181818181816567, 0.7315216790650493905 ) ) ;
#3526 = LINE ( 'NONE', #5118, #14947 ) ;
#3527 = VERTEX_POINT ( 'NONE', #9338 ) ;
#3528 = CARTESIAN_POINT ( 'NONE',  ( 2.783025336474040934, -21.08118142846912235, 12.53640742967745858 ) ) ;
#3529 = CARTESIAN_POINT ( 'NONE',  ( 1.394999999999999574, 4.147968289691286614, 27.76164181293053090 ) ) ;
#3530 = ORIENTED_EDGE ( 'NONE', *, *, #17996, .F. ) ;
#3531 = ADVANCED_FACE ( 'NONE', ( #9539 ), #7825, .F. ) ;
#3532 = DIRECTION ( 'NONE',  ( 0.000000000000000000, 0.000000000000000000, 1.000000000000000000 ) ) ;
#3533 = VECTOR ( 'NONE', #12701, 1000.000000000000000 ) ;
#3534 = CARTESIAN_POINT ( 'NONE',  ( 2.789999999999999147, -7.909232158574647009, -21.81711360614308148 ) ) ;
#3535 = CARTESIAN_POINT ( 'NONE',  ( -41.99999999999999289, -2.000000000000001776, 2.000000000000000000 ) ) ;
#3536 = VERTEX_POINT ( 'NONE', #15835 ) ;
#3537 = DIRECTION ( 'NONE',  ( -1.000000000000000000, -0.000000000000000000, -0.000000000000000000 ) ) ;
#3538 = CARTESIAN_POINT ( 'NONE',  ( 7.843749997951614539, -3.270778111535287191, -3.632567103900569361 ) ) ;
#3539 = EDGE_CURVE ( 'NONE', #725, #9066, #327, .T. ) ;
#3540 = ORIENTED_EDGE ( 'NONE', *, *, #5764, .F. ) ;
#3541 = CARTESIAN_POINT ( 'NONE',  ( 0.0003207540509381473352, -20.70663861606275447, -12.51925356660783528 ) ) ;
#3542 = ORIENTED_EDGE ( 'NONE', *, *, #5489, .F. ) ;
#3543 = APPLICATION_PROTOCOL_DEFINITION ( 'draft international standard', 'automotive_design', 1998, #17626 ) ;
#3544 = DIRECTION ( 'NONE',  ( 1.000000000000000000, 0.000000000000000000, 0.000000000000000000 ) ) ;
#3545 = CYLINDRICAL_SURFACE ( 'NONE', #633, 13.19999999999999929 ) ;
#3546 = VERTEX_POINT ( 'NONE', #17235 ) ;
#3547 = ORIENTED_EDGE ( 'NONE', *, *, #11666, .F. ) ;
#3548 = DIRECTION ( 'NONE',  ( 0.000000000000000000, 0.000000000000000000, 1.000000000000000000 ) ) ;
#3549 = DIRECTION ( 'NONE',  ( -1.000000000000000000, 0.000000000000000000, -0.000000000000000000 ) ) ;
#3550 = ORIENTED_EDGE ( 'NONE', *, *, #8918, .T. ) ;
#3551 = CARTESIAN_POINT ( 'NONE',  ( -3.846120219227901149, 3.114526743279308896, -12.34374999795161543 ) ) ;
#3552 = EDGE_CURVE ( 'NONE', #16090, #10204, #9836, .T. ) ;
#3553 = ORIENTED_EDGE ( 'NONE', *, *, #9049, .T. ) ;
#3554 = EDGE_CURVE ( 'NONE', #15613, #15969, #8218, .T. ) ;
#3555 = AXIS2_PLACEMENT_3D ( 'NONE', #12882, #18979, #5270 ) ;
#3556 = FACE_OUTER_BOUND ( 'NONE', #6096, .T. ) ;
#3557 = AXIS2_PLACEMENT_3D ( 'NONE', #12343, #15246, #18341 ) ;
#3558 = CYLINDRICAL_SURFACE ( 'NONE', #3920, 1.000000000000000888 ) ;
#3559 = CARTESIAN_POINT ( 'NONE',  ( 2.257825477245766432, -18.57583492944434411, 19.66801664102697345 ) ) ;
#3560 = EDGE_CURVE ( 'NONE', #12131, #18514, #2123, .T. ) ;
#3561 = ORIENTED_EDGE ( 'NONE', *, *, #4774, .F. ) ;
#3562 = LINE ( 'NONE', #7115, #19080 ) ;
#3563 = LINE ( 'NONE', #9687, #15746 ) ;
#3564 = EDGE_LOOP ( 'NONE', ( #18065, #15136 ) ) ;
#3565 = EDGE_LOOP ( 'NONE', ( #15916, #826 ) ) ;
#3566 = CARTESIAN_POINT ( 'NONE',  ( -30.00000000000000000, -1.925929944387235853E-31, 0.000000000000000000 ) ) ;
#3567 = ADVANCED_FACE ( 'NONE', ( #6606 ), #6405, .F. ) ;
#3568 = DIRECTION ( 'NONE',  ( 1.000000000000000000, 0.000000000000000000, 0.000000000000000000 ) ) ;
#3569 = VECTOR ( 'NONE', #12330, 1000.000000000000227 ) ;
#3570 = CARTESIAN_POINT ( 'NONE',  ( -0.5109457054261112852, 4.861323657744413218, -14.84374999795161543 ) ) ;
#3571 = CIRCLE ( 'NONE', #14760, 24.12539914357697768 ) ;
#3572 = ORIENTED_EDGE ( 'NONE', *, *, #17156, .T. ) ;
#3573 = CARTESIAN_POINT ( 'NONE',  ( 12.96874999795161543, 4.150607464521828938, -2.695436003842674566 ) ) ;
#3574 = AXIS2_PLACEMENT_3D ( 'NONE', #4612, #9315, #7897 ) ;
#3575 = CARTESIAN_POINT ( 'NONE',  ( -2.000000000000001776, 5.388445916248354013E-16, -4.400000000000000355 ) ) ;
#3576 = VERTEX_POINT ( 'NONE', #11230 ) ;
#3577 = CARTESIAN_POINT ( 'NONE',  ( 2.789999999999999147, -5.391175441198450713, -24.15498966839968276 ) ) ;
#3578 = EDGE_CURVE ( 'NONE', #11710, #4466, #17443, .T. ) ;
#3579 = CIRCLE ( 'NONE', #9023, 1.000000000000000888 ) ;
#3580 = DIRECTION ( 'NONE',  ( -0.000000000000000000, -0.000000000000000000, 1.000000000000000000 ) ) ;
#3581 = B_SPLINE_CURVE_WITH_KNOTS ( 'NONE', 3,
 ( #9732, #12526, #6592, #1722 ),
 .UNSPECIFIED., .F., .F.,
 ( 4, 4 ),
 ( 0.000000000000000000, 0.001126652051248517921 ),
 .UNSPECIFIED. ) ;
#3582 = DIRECTION ( 'NONE',  ( 1.000000000000000000, 0.000000000000000000, 0.000000000000000000 ) ) ;
#3583 = CARTESIAN_POINT ( 'NONE',  ( -2.647025296875054057, -4.584782303107560963, -6.234374998975811266 ) ) ;
#3584 = CARTESIAN_POINT ( 'NONE',  ( 5.699999999999994849, -0.9027913098498965283, -6.500000000000005329 ) ) ;
#3585 = AXIS2_PLACEMENT_3D ( 'NONE', #19400, #11804, #17907 ) ;
#3586 = EDGE_CURVE ( 'NONE', #11187, #11311, #14332, .T. ) ;
#3587 = VECTOR ( 'NONE', #17285, 1000.000000000000114 ) ;
#3588 = CARTESIAN_POINT ( 'NONE',  ( 10.47794484381774538, 0.2987243419133224775, 5.700000000000001954 ) ) ;
#3589 =( NAMED_UNIT ( * ) PLANE_ANGLE_UNIT ( ) SI_UNIT ( $, .RADIAN. ) );
#3590 = DIRECTION ( 'NONE',  ( 1.000000000000000000, 0.000000000000000000, 0.000000000000000000 ) ) ;
#3591 = AXIS2_PLACEMENT_3D ( 'NONE', #13690, #3077, #15491 ) ;
#3592 = CARTESIAN_POINT ( 'NONE',  ( 5.387740456496233676, 2.068159791354184041, -12.81249999590322552 ) ) ;
#3593 = ORIENTED_EDGE ( 'NONE', *, *, #3310, .T. ) ;
#3594 = FACE_OUTER_BOUND ( 'NONE', #5062, .T. ) ;
#3595 = PRESENTATION_STYLE_ASSIGNMENT (( #17406 ) ) ;
#3596 = CARTESIAN_POINT ( 'NONE',  ( 3.631840208645826795, 4.484949146646356688, -7.812499995903224637 ) ) ;
#3597 = ADVANCED_FACE ( 'NONE', ( #5509 ), #11433, .T. ) ;
#3598 =( GEOMETRIC_REPRESENTATION_CONTEXT ( 3 ) GLOBAL_UNCERTAINTY_ASSIGNED_CONTEXT ( ( #5770 ) ) GLOBAL_UNIT_ASSIGNED_CONTEXT ( ( #675, #19164, #18876 ) ) REPRESENTATION_CONTEXT ( 'NONE', 'WORKASPACE' ) );
#3599 = CARTESIAN_POINT ( 'NONE',  ( -2.300000000000000711, 0.000000000000000000, 0.000000000000000000 ) ) ;
#3600 = DIRECTION ( 'NONE',  ( -1.000000000000000000, -1.224646799147353207E-16, 0.000000000000000000 ) ) ;
#3601 =( BOUNDED_CURVE ( )  B_SPLINE_CURVE ( 2, ( #17413, #11502, #13100, #6880, #8301, #6785, #19194, #3698, #992, #5298, #14801, #10016, #9918, #11694, #8407, #17604, #17800 ),
 .UNSPECIFIED., .F., .F. ) 
 B_SPLINE_CURVE_WITH_KNOTS ( ( 3, 2, 2, 2, 2, 2, 2, 2, 3 ),
 ( 0.000000000000000000, 0.05000000000000000971, 0.1000000000000000194, 0.1499999999999999944, 0.2000000000000000389, 0.2500000000000000000, 0.2999999999999999889, 0.3499999999999999223, 0.4000000000000000777 ),
 .UNSPECIFIED. ) 
 CURVE ( )  GEOMETRIC_REPRESENTATION_ITEM ( )  RATIONAL_B_SPLINE_CURVE ( ( 1.000000000000000000, 0.9876883405951377704, 1.000000000000000000, 0.9876883405951377704, 1.000000000000000000, 0.9876883405951377704, 1.000000000000000000, 0.9876883405951377704, 1.000000000000000000, 0.9876883405951377704, 1.000000000000000000, 0.9876883405951377704, 1.000000000000000000, 0.9876883405951377704, 1.000000000000000000, 0.9876883405951377704, 1.000000000000000000 ) ) 
 REPRESENTATION_ITEM ( '' )  );
#3602 = VERTEX_POINT ( 'NONE', #14726 ) ;
#3603 = FACE_OUTER_BOUND ( 'NONE', #7503, .T. ) ;
#3604 = CARTESIAN_POINT ( 'NONE',  ( 1.039999999999996261, 12.96210679857786197, 24.89775460606836788 ) ) ;
#3605 = VERTEX_POINT ( 'NONE', #8433 ) ;
#3606 = CARTESIAN_POINT ( 'NONE',  ( 11.81249999590322552, -5.700000000000005507, 0.9027913098498173694 ) ) ;
#3607 = DIRECTION ( 'NONE',  ( 0.000000000000000000, 0.000000000000000000, 1.000000000000000000 ) ) ;
#3608 = AXIS2_PLACEMENT_3D ( 'NONE', #5667, #7656, #2863 ) ;
#3609 = ORIENTED_EDGE ( 'NONE', *, *, #7547, .T. ) ;
#3610 = AXIS2_PLACEMENT_3D ( 'NONE', #1931, #14141, #8134 ) ;
#3611 = AXIS2_PLACEMENT_3D ( 'NONE', #895, #2386, #19187 ) ;
#3612 = CARTESIAN_POINT ( 'NONE',  ( 2.789999999999999147, 1.991882183130632589, -24.04302995059963877 ) ) ;
#3613 = CARTESIAN_POINT ( 'NONE',  ( 7.812499995903224637, 0.9027913098498568933, -5.700000000000000178 ) ) ;
#3614 = VERTEX_POINT ( 'NONE', #4113 ) ;
#3615 = CARTESIAN_POINT ( 'NONE',  ( 0.000000000000000000, 0.000000000000000000, 37.99999999999999289 ) ) ;
#3616 = VERTEX_POINT ( 'NONE', #12934 ) ;
#3617 = CARTESIAN_POINT ( 'NONE',  ( 9.468749997951615427, -3.954556930911881985, 2.873153789725797491 ) ) ;
#3618 = VERTEX_POINT ( 'NONE', #17822 ) ;
#3619 = DIRECTION ( 'NONE',  ( 0.000000000000000000, 1.000000000000000000, 0.000000000000000000 ) ) ;
#3620 = EDGE_LOOP ( 'NONE', ( #16687, #6187, #4342, #15240, #1605, #89 ) ) ;
#3621 = CARTESIAN_POINT ( 'NONE',  ( 2.604434261026088215, -5.253342437939904741, 25.39738473784999684 ) ) ;
#3622 = EDGE_CURVE ( 'NONE', #19636, #15823, #11090, .T. ) ;
#3623 = CARTESIAN_POINT ( 'NONE',  ( 0.1882239034349760531, 12.84621645676876867, -22.54313264454999199 ) ) ;
#3624 = PRODUCT ( 'plain washer clevis pin grade a_iso_ISO 8738 - 8', 'plain washer clevis pin grade a_iso_ISO 8738 - 8', '', ( #14153 ) ) ;
#3625 = CARTESIAN_POINT ( 'NONE',  ( 2.030753610301994083, 19.12676442129372134, -19.86438386685639657 ) ) ;
#3626 = CARTESIAN_POINT ( 'NONE',  ( 1.039999999999995595, 20.02152543075345648, 19.67366047555537278 ) ) ;
#3627 = ORIENTED_EDGE ( 'NONE', *, *, #7968, .T. ) ;
#3628 = FACE_BOUND ( 'NONE', #15050, .T. ) ;
#3629 = DIRECTION ( 'NONE',  ( 0.000000000000000000, 0.000000000000000000, 1.000000000000000000 ) ) ;
#3630 = ORIENTED_EDGE ( 'NONE', *, *, #2598, .T. ) ;
#3631 = EDGE_CURVE ( 'NONE', #7114, #5932, #11687, .T. ) ;
#3632 =( GEOMETRIC_REPRESENTATION_CONTEXT ( 3 ) GLOBAL_UNCERTAINTY_ASSIGNED_CONTEXT ( ( #1185 ) ) GLOBAL_UNIT_ASSIGNED_CONTEXT ( ( #18893, #8584, #3986 ) ) REPRESENTATION_CONTEXT ( 'NONE', 'WORKASPACE' ) );
#3633 = CARTESIAN_POINT ( 'NONE',  ( -11.32184790671638730, 13.12143529358541549, -35.00000000000000000 ) ) ;
#3634 = DIRECTION ( 'NONE',  ( 1.000000000000000000, 0.000000000000000000, 0.000000000000000000 ) ) ;
#3635 = CARTESIAN_POINT ( 'NONE',  ( -0.5109457054262123155, -4.861323657744403448, -8.468749997951615427 ) ) ;
#3636 = ORIENTED_EDGE ( 'NONE', *, *, #1303, .F. ) ;
#3637 = CARTESIAN_POINT ( 'NONE',  ( -15.00000000000000355, -4.215373648918917304, -3.375000000000002220 ) ) ;
#3638 = ADVANCED_FACE ( 'NONE', ( #830 ), #11718, .F. ) ;
#3639 = CARTESIAN_POINT ( 'NONE',  ( 8.312499995903225525, -3.814044456245443193, -4.235925505221191933 ) ) ;
#3640 = DIRECTION ( 'NONE',  ( 1.000000000000000000, 0.000000000000000000, 0.000000000000000000 ) ) ;
#3641 = VECTOR ( 'NONE', #10871, 1000.000000000000000 ) ;
#3642 = ORIENTED_EDGE ( 'NONE', *, *, #5348, .T. ) ;
#3643 = CARTESIAN_POINT ( 'NONE',  ( -7.722669826818730404E-14, -20.65026423218563778, -12.51972477286604502 ) ) ;
#3644 = ORIENTED_EDGE ( 'NONE', *, *, #5582, .F. ) ;
#3645 = CARTESIAN_POINT ( 'NONE',  ( 6.843749997951615427, 4.233219804643871598, 2.444050593750020095 ) ) ;
#3646 = CARTESIAN_POINT ( 'NONE',  ( 10.84374999795161543, 3.632567103900523620, 3.270778111535338262 ) ) ;
#3647 = ORIENTED_EDGE ( 'NONE', *, *, #11378, .F. ) ;
#3648 = ORIENTED_EDGE ( 'NONE', *, *, #1885, .F. ) ;
#3649 = CARTESIAN_POINT ( 'NONE',  ( 3.968750000000004441, -6.874076642538978987, 0.000000000000000000 ) ) ;
#3650 = CARTESIAN_POINT ( 'NONE',  ( 4.465502636338025688, -1.988169868018592412, -14.84374999795161543 ) ) ;
#3651 =( GEOMETRIC_REPRESENTATION_CONTEXT ( 3 ) GLOBAL_UNCERTAINTY_ASSIGNED_CONTEXT ( ( #19587 ) ) GLOBAL_UNIT_ASSIGNED_CONTEXT ( ( #4281, #8785, #13380 ) ) REPRESENTATION_CONTEXT ( 'NONE', 'WORKASPACE' ) );
#3652 = CIRCLE ( 'NONE', #17105, 4.000000000000000000 ) ;
#3653 = DIRECTION ( 'NONE',  ( 1.000000000000000000, 0.000000000000000000, 0.000000000000000000 ) ) ;
#3654 = ORIENTED_EDGE ( 'NONE', *, *, #16122, .T. ) ;
#3655 = EDGE_CURVE ( 'NONE', #13831, #6807, #567, .T. ) ;
#3656 = CIRCLE ( 'NONE', #11652, 8.073750000000021743 ) ;
#3657 = EDGE_LOOP ( 'NONE', ( #4335, #1929, #18345, #15145 ) ) ;
#3658 = LINE ( 'NONE', #18764, #5710 ) ;
#3659 = PLANE ( 'NONE',  #2970 ) ;
#3660 = FACE_BOUND ( 'NONE', #5050, .T. ) ;
#3661 = ORIENTED_EDGE ( 'NONE', *, *, #16689, .F. ) ;
#3662 = CARTESIAN_POINT ( 'NONE',  ( 0.5321745379877909077, -23.74442027961350377, -12.96514671151793507 ) ) ;
#3663 = CARTESIAN_POINT ( 'NONE',  ( 0.9661342547375842971, -24.74813374239834474, 12.96725027898183669 ) ) ;
#3664 = VECTOR ( 'NONE', #3590, 1000.000000000000000 ) ;
#3665 = ORIENTED_EDGE ( 'NONE', *, *, #5162, .F. ) ;
#3666 = EDGE_CURVE ( 'NONE', #6695, #7627, #14290, .T. ) ;
#3667 = EDGE_CURVE ( 'NONE', #18545, #3927, #15024, .T. ) ;
#3668 = ORIENTED_EDGE ( 'NONE', *, *, #2017, .F. ) ;
#3669 = CARTESIAN_POINT ( 'NONE',  ( -4.620319390059805187, 1.773574444220790136, -10.96874999795161720 ) ) ;
#3670 = LINE ( 'NONE', #8175, #4878 ) ;
#3671 = EDGE_CURVE ( 'NONE', #411, #1533, #5321, .T. ) ;
#3672 = AXIS2_PLACEMENT_3D ( 'NONE', #13943, #3232, #236 ) ;
#3673 = FACE_OUTER_BOUND ( 'NONE', #17019, .T. ) ;
#3674 = ORIENTED_EDGE ( 'NONE', *, *, #13292, .T. ) ;
#3675 = DIRECTION ( 'NONE',  ( 1.000000000000000000, 0.000000000000000000, 0.000000000000000000 ) ) ;
#3676 = CARTESIAN_POINT ( 'NONE',  ( 8.812499995903225525, -3.143139765844555900, -4.840010801796527318 ) ) ;
#3677 = ORIENTED_EDGE ( 'NONE', *, *, #13115, .T. ) ;
#3678 = CARTESIAN_POINT ( 'NONE',  ( 1.394999999999999574, 20.02152543075346003, 19.67366047555537634 ) ) ;
#3679 = FACE_OUTER_BOUND ( 'NONE', #4476, .T. ) ;
#3680 = APPLICATION_CONTEXT ( 'automotive_design' ) ;
#3681 = CARTESIAN_POINT ( 'NONE',  ( 2.031033491000346913, -12.05173163741705444, -24.80232951178391332 ) ) ;
#3682 = CARTESIAN_POINT ( 'NONE',  ( 2.765633920072241292, 18.55949924794916228, -16.37294372382838148 ) ) ;
#3683 = CARTESIAN_POINT ( 'NONE',  ( 5.700000000000001954, 0.2987243419133224775, -9.165444847914525184 ) ) ;
#3684 = VECTOR ( 'NONE', #18301, 1000.000000000000000 ) ;
#3685 = DIRECTION ( 'NONE',  ( 0.000000000000000000, 0.000000000000000000, 1.000000000000000000 ) ) ;
#3686 = FILL_AREA_STYLE_COLOUR ( '', #7128 ) ;
#3687 = DIRECTION ( 'NONE',  ( 0.000000000000000000, 0.000000000000000000, 1.000000000000000000 ) ) ;
#3688 = CIRCLE ( 'NONE', #10100, 6.543750000000017941 ) ;
#3689 = CARTESIAN_POINT ( 'NONE',  ( 2.318398865532073749, 5.207209108562820710, -10.31249999590322552 ) ) ;
#3690 = VERTEX_POINT ( 'NONE', #1009 ) ;
#3691 = DIRECTION ( 'NONE',  ( 0.000000000000000000, 0.000000000000000000, 1.000000000000000000 ) ) ;
#3692 = CARTESIAN_POINT ( 'NONE',  ( 2.031033491000347357, 12.05173163741723030, 24.80232951178382805 ) ) ;
#3693 = CARTESIAN_POINT ( 'NONE',  ( 4.861323657744411442, 0.5109457054261445919, -9.843749997951615427 ) ) ;
#3694 = CARTESIAN_POINT ( 'NONE',  ( 13.00000000000000533, -5.207209108562836697, 2.318398865532038666 ) ) ;
#3695 = CARTESIAN_POINT ( 'NONE',  ( 8.343749997951611874, -4.942249507334558700, 0.2590123213420631454 ) ) ;
#3696 = EDGE_LOOP ( 'NONE', ( #9432, #2129, #2748, #4857 ) ) ;
#3697 = CARTESIAN_POINT ( 'NONE',  ( -25.31088913245550032, 24.69615242270646149, 37.99999999999999289 ) ) ;
#3698 = CARTESIAN_POINT ( 'NONE',  ( -2.695436003842760719, -4.150607464521772094, -10.34374999795161543 ) ) ;
#3699 = ORIENTED_EDGE ( 'NONE', *, *, #6386, .T. ) ;
#3700 = EDGE_CURVE ( 'NONE', #17330, #4658, #14705, .T. ) ;
#3701 = CARTESIAN_POINT ( 'NONE',  ( 2.789999999999999147, 9.836394144775706394, 22.71065055754456097 ) ) ;
#3702 = EDGE_CURVE ( 'NONE', #12760, #9739, #8535, .T. ) ;
#3703 = DIRECTION ( 'NONE',  ( -1.000000000000000000, 0.000000000000000000, 0.000000000000000000 ) ) ;
#3704 = ORIENTED_EDGE ( 'NONE', *, *, #2467, .F. ) ;
#3705 = DIRECTION ( 'NONE',  ( -1.000000000000000000, -0.000000000000000000, 0.000000000000000000 ) ) ;
#3706 = AXIS2_PLACEMENT_3D ( 'NONE', #14926, #10135, #928 ) ;
#3707 = CARTESIAN_POINT ( 'NONE',  ( -14.19790265903626647, 9.644882309621941374, 32.00000000000000000 ) ) ;
#3708 = EDGE_CURVE ( 'NONE', #15591, #18627, #13604, .T. ) ;
#3709 = DIRECTION ( 'NONE',  ( -0.000000000000000000, -0.000000000000000000, 1.000000000000000000 ) ) ;
#3710 = CARTESIAN_POINT ( 'NONE',  ( 0.000000000000000000, 1.991882183130315953, 24.04302995059967074 ) ) ;
#3711 = ORIENTED_EDGE ( 'NONE', *, *, #14684, .F. ) ;
#3712 = CARTESIAN_POINT ( 'NONE',  ( 9.580134541264516912, -14.56230589874905412, 32.00000000000000000 ) ) ;
#3713 =( NAMED_UNIT ( * ) PLANE_ANGLE_UNIT ( ) SI_UNIT ( $, .RADIAN. ) );
#3714 = DIRECTION ( 'NONE',  ( -0.000000000000000000, 0.000000000000000000, 1.000000000000000000 ) ) ;
#3715 = EDGE_LOOP ( 'NONE', ( #17033, #2708, #10778, #8562 ) ) ;
#3716 = DIRECTION ( 'NONE',  ( 1.000000000000000000, 3.873737557103174326E-15, 0.000000000000000000 ) ) ;
#3717 = VERTEX_POINT ( 'NONE', #10038 ) ;
#3718 = EDGE_CURVE ( 'NONE', #3097, #1526, #18121, .T. ) ;
#3719 = DIRECTION ( 'NONE',  ( 1.000000000000000000, 0.000000000000000000, 0.000000000000000000 ) ) ;
#3720 = VECTOR ( 'NONE', #2307, 1000.000000000000000 ) ;
#3721 = ORIENTED_EDGE ( 'NONE', *, *, #7803, .T. ) ;
#3722 = EDGE_CURVE ( 'NONE', #17625, #10948, #5699, .T. ) ;
#3723 = DIRECTION ( 'NONE',  ( 0.000000000000000000, 0.000000000000000000, -1.000000000000000000 ) ) ;
#3724 = AXIS2_PLACEMENT_3D ( 'NONE', #5371, #785, #6960 ) ;
#3725 = CARTESIAN_POINT ( 'NONE',  ( -5.700000000000000178, 0.9027913098498568933, -7.812499995903224637 ) ) ;
#3726 = LINE ( 'NONE', #8228, #9649 ) ;
#3727 = CARTESIAN_POINT ( 'NONE',  ( -7.937500000000000000, 0.000000000000000000, 0.000000000000000000 ) ) ;
#3728 = VERTEX_POINT ( 'NONE', #8914 ) ;
#3729 = CARTESIAN_POINT ( 'NONE',  ( 6.843749997951615427, 4.233219804643887585, -2.444050593749990785 ) ) ;
#3730 = DIRECTION ( 'NONE',  ( 1.000000000000000000, 0.000000000000000000, 0.000000000000000000 ) ) ;
#3731 = VERTEX_POINT ( 'NONE', #19508 ) ;
#3732 = CIRCLE ( 'NONE', #15235, 28.06981291497571007 ) ;
#3733 = CARTESIAN_POINT ( 'NONE',  ( 2.789999999999999147, 0.2301004812057544924, 24.44424927289185590 ) ) ;
#3734 = VECTOR ( 'NONE', #1828, 1000.000000000000000 ) ;
#3735 = ADVANCED_FACE ( 'NONE', ( #9013 ), #16627, .F. ) ;
#3736 = CARTESIAN_POINT ( 'NONE',  ( 2.601776105308176934, 2.857713464479052057, -25.78859396478524957 ) ) ;
#3737 = CARTESIAN_POINT ( 'NONE',  ( -10.99900000000000233, -7.061101152771736665E-32, 0.000000000000000000 ) ) ;
#3738 = ORIENTED_EDGE ( 'NONE', *, *, #11268, .F. ) ;
#3739 = CARTESIAN_POINT ( 'NONE',  ( 0.02436607992776021470, 21.30679549418649543, -12.59161484032888723 ) ) ;
#3740 = CARTESIAN_POINT ( 'NONE',  ( 4.888101187500000222, -3.413342815706642518E-14, -6.468749997951615427 ) ) ;
#3741 = DIRECTION ( 'NONE',  ( 1.000000000000000000, -0.000000000000000000, -0.000000000000000000 ) ) ;
#3742 = ORIENTED_EDGE ( 'NONE', *, *, #1879, .F. ) ;
#3743 = DIRECTION ( 'NONE',  ( 1.000000000000000000, 0.000000000000000000, 0.000000000000000000 ) ) ;
#3744 = EDGE_CURVE ( 'NONE', #16939, #7007, #4705, .T. ) ;
#3745 = ORIENTED_EDGE ( 'NONE', *, *, #9552, .T. ) ;
#3746 = CONTEXT_DEPENDENT_SHAPE_REPRESENTATION ( #19193, #7289 ) ;
#3747 = FACE_OUTER_BOUND ( 'NONE', #18882, .T. ) ;
#3748 = CARTESIAN_POINT ( 'NONE',  ( -17.28688694438836393, -7.664027248171298545, 32.00000000000000000 ) ) ;
#3749 = ORIENTED_EDGE ( 'NONE', *, *, #8444, .F. ) ;
#3750 = VERTEX_POINT ( 'NONE', #15018 ) ;
#3751 = CARTESIAN_POINT ( 'NONE',  ( 0.000000000000000000, 5.535312321042724193, 23.48180575137730841 ) ) ;
#3752 = CARTESIAN_POINT ( 'NONE',  ( 6.000000000000005329, 0.000000000000000000, 0.000000000000000000 ) ) ;
#3753 = AXIS2_PLACEMENT_3D ( 'NONE', #10349, #5919, #19434 ) ;
#3754 = CARTESIAN_POINT ( 'NONE',  ( 3.968750000000004441, -6.874076642538978987, 0.000000000000000000 ) ) ;
#3755 = AXIS2_PLACEMENT_3D ( 'NONE', #856, #5633, #5727 ) ;
#3756 = EDGE_LOOP ( 'NONE', ( #13695, #6353, #8426, #17868, #16338, #14629 ) ) ;
#3757 = ADVANCED_FACE ( 'NONE', ( #5902 ), #10715, .F. ) ;
#3758 = CARTESIAN_POINT ( 'NONE',  ( -36.00000000000000000, -6.000000000000000888, 7.347880794884120722E-16 ) ) ;
#3759 = ORIENTED_EDGE ( 'NONE', *, *, #4413, .F. ) ;
#3760 = B_SPLINE_CURVE_WITH_KNOTS ( 'NONE', 3,
 ( #16702, #13694, #7578, #10597 ),
 .UNSPECIFIED., .F., .F.,
 ( 4, 4 ),
 ( 0.005258120783916810613, 0.005948386350302961936 ),
 .UNSPECIFIED. ) ;
#3761 = ADVANCED_FACE ( 'NONE', ( #4408 ), #9217, .T. ) ;
#3762 = VECTOR ( 'NONE', #18432, 1000.000000000000000 ) ;
#3763 = DIRECTION ( 'NONE',  ( 1.000000000000000000, 0.000000000000000000, 0.000000000000000000 ) ) ;
#3764 = FACE_OUTER_BOUND ( 'NONE', #3355, .T. ) ;
#3765 = CARTESIAN_POINT ( 'NONE',  ( -3.114526743279308896, -3.846120219227901149, -6.968749997951614539 ) ) ;
#3766 = ORIENTED_EDGE ( 'NONE', *, *, #14831, .T. ) ;
#3767 = EDGE_CURVE ( 'NONE', #2770, #6039, #18221, .T. ) ;
#3768 = EDGE_LOOP ( 'NONE', ( #11132, #10471, #6114, #17257 ) ) ;
#3769 = ORIENTED_EDGE ( 'NONE', *, *, #16974, .T. ) ;
#3770 = CARTESIAN_POINT ( 'NONE',  ( -5.763142191869152775, 0.3020334839683282979, -9.500000000000003553 ) ) ;
#3771 = CARTESIAN_POINT ( 'NONE',  ( 0.000000000000000000, 0.000000000000000000, 0.000000000000000000 ) ) ;
#3772 = VECTOR ( 'NONE', #1798, 1000.000000000000000 ) ;
#3773 = CARTESIAN_POINT ( 'NONE',  ( 6.626241948324199882, -16.73597674598852691, -32.00000000000000000 ) ) ;
#3774 = ORIENTED_EDGE ( 'NONE', *, *, #16433, .F. ) ;
#3775 = DIRECTION ( 'NONE',  ( 0.000000000000000000, 0.000000000000000000, 1.000000000000000000 ) ) ;
#3776 = CARTESIAN_POINT ( 'NONE',  ( 8.343749997951613651, -2.695436003842674122, -4.150607464521828938 ) ) ;
#3777 = ORIENTED_EDGE ( 'NONE', *, *, #353, .T. ) ;
#3778 = DIRECTION ( 'NONE',  ( -1.000000000000000000, 0.000000000000000000, 0.000000000000000000 ) ) ;
#3779 = EDGE_CURVE ( 'NONE', #17931, #2783, #15894, .T. ) ;
#3780 = CYLINDRICAL_SURFACE ( 'NONE', #2905, 4.200000000000000178 ) ;
#3781 = CARTESIAN_POINT ( 'NONE',  ( -20.63749999999999929, 0.000000000000000000, -4.824999999999999289 ) ) ;
#3782 = CARTESIAN_POINT ( 'NONE',  ( 1.960886852992457241, 24.44424927289185945, 12.96989951879416125 ) ) ;
#3783 = CARTESIAN_POINT ( 'NONE',  ( 0.000000000000000000, 0.000000000000000000, -0.6113687067993561763 ) ) ;
#3784 = AXIS2_PLACEMENT_3D ( 'NONE', #11665, #7237, #13362 ) ;
#3785 = FACE_OUTER_BOUND ( 'NONE', #1825, .T. ) ;
#3786 =( LENGTH_UNIT ( ) NAMED_UNIT ( * ) SI_UNIT ( .MILLI., .METRE. ) );
#3787 = DIRECTION ( 'NONE',  ( 0.000000000000000000, 1.374038396813314756E-15, -1.000000000000000000 ) ) ;
#3788 = EDGE_CURVE ( 'NONE', #8597, #10842, #12707, .T. ) ;
#3789 = ORIENTED_EDGE ( 'NONE', *, *, #10519, .T. ) ;
#3790 = FACE_OUTER_BOUND ( 'NONE', #14284, .T. ) ;
#3791 = CARTESIAN_POINT ( 'NONE',  ( 1.394999999999999574, 4.147968289691677413, -27.76164181293047761 ) ) ;
#3792 = UNCERTAINTY_MEASURE_WITH_UNIT (LENGTH_MEASURE( 1.000000000000000082E-05 ), #10030, 'distance_accuracy_value', 'NONE');
#3793 = CARTESIAN_POINT ( 'NONE',  ( -90.00000000000000000, 9.887492094615969966E-16, 8.073750000000021743 ) ) ;
#3794 = B_SPLINE_CURVE_WITH_KNOTS ( 'NONE', 3,
 ( #7782, #13894, #7149, #8383, #685, #11775, #6859, #8669, #17584, #17780 ),
 .UNSPECIFIED., .F., .F.,
 ( 4, 3, 3, 4 ),
 ( 0.000000000000000000, 0.0001875345074742634278, 0.0003808595644229697272, 0.0005744879655065562602 ),
 .UNSPECIFIED. ) ;
#3795 = CARTESIAN_POINT ( 'NONE',  ( 9.343749997951615427, -4.780397808154247308, -1.280903732194487166 ) ) ;
#3796 = CARTESIAN_POINT ( 'NONE',  ( 0.07181525696555295102, -5.344212458769539431, 24.78695292654919768 ) ) ;
#3797 = CARTESIAN_POINT ( 'NONE',  ( -2.246813503491833508, 4.409619785863906571, -10.34374999795161543 ) ) ;
#3798 = ORIENTED_EDGE ( 'NONE', *, *, #14971, .F. ) ;
#3799 = FACE_OUTER_BOUND ( 'NONE', #15750, .T. ) ;
#3800 = CARTESIAN_POINT ( 'NONE',  ( 0.02436607992776628623, 24.63872515616082737, -2.336989772644355590 ) ) ;
#3801 = CIRCLE ( 'NONE', #8916, 9.000000000000000000 ) ;
#3802 = VERTEX_POINT ( 'NONE', #18699 ) ;
#3803 = CARTESIAN_POINT ( 'NONE',  ( -3.968750000000004441, 6.874076642538978987, 0.000000000000000000 ) ) ;
#3804 = EDGE_CURVE ( 'NONE', #7952, #3208, #5936, .T. ) ;
#3805 = CARTESIAN_POINT ( 'NONE',  ( 1.039999999999996483, 4.147968289691283950, 27.76164181293052735 ) ) ;
#3806 = PRODUCT_DEFINITION_FORMATION_WITH_SPECIFIED_SOURCE ( 'ANY', '', #4114, .NOT_KNOWN. ) ;
#3807 = CARTESIAN_POINT ( 'NONE',  ( -4.999999999999966249, -7.196152422706654228, 37.99999999999999289 ) ) ;
#3808 = DIRECTION ( 'NONE',  ( 0.000000000000000000, 0.000000000000000000, -1.000000000000000000 ) ) ;
#3809 = ORIENTED_EDGE ( 'NONE', *, *, #18728, .F. ) ;
#3810 = FACE_OUTER_BOUND ( 'NONE', #9635, .T. ) ;
#3811 = DIRECTION ( 'NONE',  ( 0.000000000000000000, 0.000000000000000000, 1.000000000000000000 ) ) ;
#3812 = EDGE_CURVE ( 'NONE', #3717, #10033, #8362, .T. ) ;
#3813 = VERTEX_POINT ( 'NONE', #5091 ) ;
#3814 = CARTESIAN_POINT ( 'NONE',  ( 13.96874999795161365, -3.499494075959791672, -3.499494075959840078 ) ) ;
#3815 = ORIENTED_EDGE ( 'NONE', *, *, #777, .T. ) ;
#3816 = ADVANCED_FACE ( 'NONE', ( #11204 ), #7993, .F. ) ;
#3817 = CARTESIAN_POINT ( 'NONE',  ( 2.765633920072241736, -9.836394144775550075, -22.71065055754462492 ) ) ;
#3818 = ORIENTED_EDGE ( 'NONE', *, *, #17472, .F. ) ;
#3819 = CARTESIAN_POINT ( 'NONE',  ( 2.262072661820536901, 3.461047254864260125, 26.82026385750179287 ) ) ;
#3820 = CARTESIAN_POINT ( 'NONE',  ( -4.611396867937201272, 3.350375938067097437, -9.312499995903225525 ) ) ;
#3821 = CARTESIAN_POINT ( 'NONE',  ( 2.718184757033982546, 16.91181672897760535, -18.89296398180173497 ) ) ;
#3822 = CARTESIAN_POINT ( 'NONE',  ( 7.312499995903225525, 4.936344801571289409, 2.850000000000024070 ) ) ;
#3823 = VERTEX_POINT ( 'NONE', #9313 ) ;
#3824 = CARTESIAN_POINT ( 'NONE',  ( 0.2590123213420631454, -4.942249507334558700, -8.343749997951611874 ) ) ;
#3825 = EDGE_CURVE ( 'NONE', #13278, #9359, #19068, .T. ) ;
#3826 = FACE_OUTER_BOUND ( 'NONE', #17914, .T. ) ;
#3827 = VERTEX_POINT ( 'NONE', #16921 ) ;
#3828 = CARTESIAN_POINT ( 'NONE',  ( -12.86923836996420611, -11.47363181547641275, 32.00000000000000000 ) ) ;
#3830 = EDGE_CURVE ( 'NONE', #3750, #1741, #8096, .T. ) ;
#3829 = ADVANCED_FACE ( 'NONE', ( #13912 ), #9500, .T. ) ;
#3831 = CARTESIAN_POINT ( 'NONE',  ( 0.000000000000000000, 0.000000000000000000, 0.000000000000000000 ) ) ;
#3832 = CYLINDRICAL_SURFACE ( 'NONE', #4896, 1.000000000000000000 ) ;
#3833 = EDGE_LOOP ( 'NONE', ( #10273, #1506 ) ) ;
#3835 = CARTESIAN_POINT ( 'NONE',  ( 2.789999999999999147, -15.04425356660774682, 20.70663861606266209 ) ) ;
#3834 = AXIS2_PLACEMENT_3D ( 'NONE', #19529, #4524, #13336 ) ;
#3836 = DIRECTION ( 'NONE',  ( 0.000000000000000000, 0.000000000000000000, -1.000000000000000000 ) ) ;
#3837 = CIRCLE ( 'NONE', #2552, 6.000000000000000000 ) ;
#3838 = CARTESIAN_POINT ( 'NONE',  ( 0.02436607992775978102, 2.336989772644613161, -24.63872515616080250 ) ) ;
#3839 = ORIENTED_EDGE ( 'NONE', *, *, #1838, .F. ) ;
#3840 = CARTESIAN_POINT ( 'NONE',  ( -10.58013454126452224, -14.56230589874905235, 32.00000000000000000 ) ) ;
#3841 = ORIENTED_EDGE ( 'NONE', *, *, #8446, .F. ) ;
#3842 = ITEM_DEFINED_TRANSFORMATION ( 'NONE', 'NONE', #296,  #16724 ) ;
#3843 = CARTESIAN_POINT ( 'NONE',  ( 9.343749997951615427, 1.280903732194421218, 4.780397808154266848 ) ) ;
#3844 = CARTESIAN_POINT ( 'NONE',  ( -0.8944271909999155223, 0.000000000000000000, -5.200000000000000178 ) ) ;
#3845 = CARTESIAN_POINT ( 'NONE',  ( 2.789999999999999147, -23.31896751603326834, -7.334849878007764445 ) ) ;
#3846 = VERTEX_POINT ( 'NONE', #9610 ) ;
#3847 = CARTESIAN_POINT ( 'NONE',  ( 1.510506337161829027, -4.648860486681964055, -10.84374999795161543 ) ) ;
#3848 = CYLINDRICAL_SURFACE ( 'NONE', #10723, 5.700000000000001954 ) ;
#3849 = DIRECTION ( 'NONE',  ( 0.000000000000000000, 0.000000000000000000, -1.000000000000000000 ) ) ;
#3850 = ORIENTED_EDGE ( 'NONE', *, *, #5946, .T. ) ;
#3851 = AXIS2_PLACEMENT_3D ( 'NONE', #10591, #17894, #13386 ) ;
#3852 = AXIS2_PLACEMENT_3D ( 'NONE', #4700, #18406, #18695 ) ;
#3853 = CARTESIAN_POINT ( 'NONE',  ( -2.695436003842674122, 4.150607464521828938, -13.34374999795161365 ) ) ;
#3854 = ORIENTED_EDGE ( 'NONE', *, *, #11239, .T. ) ;
#3855 = B_SPLINE_CURVE_WITH_KNOTS ( 'NONE', 3,
 ( #9751, #15842, #11040, #12546 ),
 .UNSPECIFIED., .F., .F.,
 ( 4, 4 ),
 ( 0.005258105385878685673, 0.005948373736081384068 ),
 .UNSPECIFIED. ) ;
#3856 = DIRECTION ( 'NONE',  ( -0.000000000000000000, -0.000000000000000000, 1.000000000000000000 ) ) ;
#3857 = CARTESIAN_POINT ( 'NONE',  ( 9.000000000000000000, 0.000000000000000000, 29.00000000000000355 ) ) ;
#3858 = ORIENTED_EDGE ( 'NONE', *, *, #11932, .F. ) ;
#3859 = CARTESIAN_POINT ( 'NONE',  ( -1.280903732194386802, 4.780397808154273065, -13.96874999795161365 ) ) ;
#3860 =( REPRESENTATION_RELATIONSHIP ('NONE','NONE', #18211, #11438 ) REPRESENTATION_RELATIONSHIP_WITH_TRANSFORMATION ( #3842 )SHAPE_REPRESENTATION_RELATIONSHIP( ) );
#3861 =( NAMED_UNIT ( * ) SI_UNIT ( $, .STERADIAN. ) SOLID_ANGLE_UNIT ( ) );
#3862 = LINE ( 'NONE', #8474, #10012 ) ;
#3863 = ORIENTED_EDGE ( 'NONE', *, *, #9847, .F. ) ;
#3864 = ORIENTED_EDGE ( 'NONE', *, *, #16085, .F. ) ;
#3865 = CARTESIAN_POINT ( 'NONE',  ( -4.484949146646330931, 3.631840208645857437, -11.50000000000000355 ) ) ;
#3866 = DIRECTION ( 'NONE',  ( -1.000000000000000000, -0.000000000000000000, 0.000000000000000000 ) ) ;
#3867 = DIRECTION ( 'NONE',  ( 1.000000000000000000, 0.000000000000000000, 0.000000000000000000 ) ) ;
#3868 = VERTEX_POINT ( 'NONE', #302 ) ;
#3869 = CARTESIAN_POINT ( 'NONE',  ( 14.84374999795161543, 4.861323657744413218, -0.5109457054261112852 ) ) ;
#3870 = CARTESIAN_POINT ( 'NONE',  ( 7.812499995903224637, -4.484949146646330931, -3.631840208645857437 ) ) ;
#3871 = CIRCLE ( 'NONE', #6412, 8.265000000000021885 ) ;
#3872 = ORIENTED_EDGE ( 'NONE', *, *, #16483, .T. ) ;
#3873 = CARTESIAN_POINT ( 'NONE',  ( 0.000000000000000000, 0.000000000000000000, 0.000000000000000000 ) ) ;
#3874 = AXIS2_PLACEMENT_3D ( 'NONE', #12938, #17632, #5226 ) ;
#3875 = EDGE_CURVE ( 'NONE', #5549, #2241, #1897, .T. ) ;
#3876 = AXIS2_PLACEMENT_3D ( 'NONE', #17878, #1171, #4169 ) ;
#3877 = CARTESIAN_POINT ( 'NONE',  ( 1.869200000000000195, 0.000000000000000000, -6.760799999999997034 ) ) ;
#3878 = CARTESIAN_POINT ( 'NONE',  ( -0.2436698586202288019, 0.000000000000000000, 0.000000000000000000 ) ) ;
#3879 = CARTESIAN_POINT ( 'NONE',  ( 2.601776091974069782, -25.40949241676357317, 5.251266773802275800 ) ) ;
#3880 = DIRECTION ( 'NONE',  ( 1.000000000000000000, 0.000000000000000000, 0.000000000000000000 ) ) ;
#3881 = SHAPE_REPRESENTATION_RELATIONSHIP ( 'NONE' , 'NONE' ,  #10045, #17347 ) ;
#3882 = DIRECTION ( 'NONE',  ( 0.000000000000000000, 0.000000000000000000, 1.000000000000000000 ) ) ;
#3883 = SURFACE_STYLE_USAGE ( .BOTH. , #11303 ) ;
#3884 = ORIENTED_EDGE ( 'NONE', *, *, #3830, .T. ) ;
#3885 =( BOUNDED_CURVE ( )  B_SPLINE_CURVE ( 2, ( #9257, #2112, #17323, #19020, #9157, #8216, #11221, #12922, #9631, #15724, #18819 ),
 .UNSPECIFIED., .F., .F. ) 
 B_SPLINE_CURVE_WITH_KNOTS ( ( 3, 2, 2, 2, 2, 3 ),
 ( 0.1666819079834106210, 0.2000000000000000111, 0.2500000000000000000, 0.2999999999999999889, 0.3499999999999999778, 0.4000000000000000222 ),
 .UNSPECIFIED. ) 
 CURVE ( )  GEOMETRIC_REPRESENTATION_ITEM ( )  RATIONAL_B_SPLINE_CURVE ( ( 0.9945256517182514688, 0.9917959799814378696, 1.000000000000000000, 0.9876883405951377704, 1.000000000000000000, 0.9876883405951377704, 1.000000000000000000, 0.9876883405951377704, 1.000000000000000000, 0.9876883405951377704, 1.000000000000000000 ) ) 
 REPRESENTATION_ITEM ( '' )  );
#3886 = CYLINDRICAL_SURFACE ( 'NONE', #2170, 4.824999999999999289 ) ;
#3887 = AXIS2_PLACEMENT_3D ( 'NONE', #14712, #7079, #17711 ) ;
#3888 = LINE ( 'NONE', #19385, #756 ) ;
#3889 = FACE_OUTER_BOUND ( 'NONE', #5653, .T. ) ;
#3890 = CIRCLE ( 'NONE', #14444, 1.000000000000000000 ) ;
#3891 = CARTESIAN_POINT ( 'NONE',  ( -36.00000000000000000, -5.000000000000000888, 5.000000000000000000 ) ) ;
#3892 = CARTESIAN_POINT ( 'NONE',  ( 0.5321745407694777885, -4.993157874728001211, 26.58873630738050409 ) ) ;
#3893 = B_SPLINE_CURVE_WITH_KNOTS ( 'NONE', 3,
 ( #9420, #7998, #12712, #15811 ),
 .UNSPECIFIED., .F., .F.,
 ( 4, 4 ),
 ( 0.005342776758202895035, 0.005948405594583416715 ),
 .UNSPECIFIED. ) ;
#3894 = CARTESIAN_POINT ( 'NONE',  ( 3.499494075959815653, 3.499494075959816541, -14.34374999795161543 ) ) ;
#3895 = ORIENTED_EDGE ( 'NONE', *, *, #1258, .F. ) ;
#3896 = CARTESIAN_POINT ( 'NONE',  ( 8.843749997951615427, -2.873153789725853002, 3.954556930911842016 ) ) ;
#3897 = PLANE ( 'NONE',  #7220 ) ;
#3898 = ORIENTED_EDGE ( 'NONE', *, *, #8109, .T. ) ;
#3899 = CARTESIAN_POINT ( 'NONE',  ( 9.580134541264516912, -14.56230589874905412, -32.00000000000000000 ) ) ;
#3900 = EDGE_CURVE ( 'NONE', #11206, #6326, #15709, .T. ) ;
#3901 = DIRECTION ( 'NONE',  ( -1.000000000000000000, 0.000000000000000000, 0.000000000000000000 ) ) ;
#3902 = AXIS2_PLACEMENT_3D ( 'NONE', #16015, #8418, #11512 ) ;
#3903 = CIRCLE ( 'NONE', #7395, 1.000000000000002665 ) ;
#3904 = AXIS2_PLACEMENT_3D ( 'NONE', #14181, #6453, #17580 ) ;
#3905 = LINE ( 'NONE', #19016, #7737 ) ;
#3906 = LINE ( 'NONE', #5689, #18014 ) ;
#3907 = EDGE_LOOP ( 'NONE', ( #15439, #5683, #14430, #10674 ) ) ;
#3908 = DIRECTION ( 'NONE',  ( 0.000000000000000000, 0.000000000000000000, 1.000000000000000000 ) ) ;
#3909 = DIRECTION ( 'NONE',  ( 0.000000000000000000, 0.000000000000000000, 1.000000000000000000 ) ) ;
#3910 = AXIS2_PLACEMENT_3D ( 'NONE', #1575, #13381, #1281 ) ;
#3911 = DIRECTION ( 'NONE',  ( 0.000000000000000000, 0.000000000000000000, -1.000000000000000000 ) ) ;
#3912 = ORIENTED_EDGE ( 'NONE', *, *, #19038, .F. ) ;
#3913 = CARTESIAN_POINT ( 'NONE',  ( 2.789999999999999147, 18.55949924794892780, 16.37294372382865504 ) ) ;
#3914 = VERTEX_POINT ( 'NONE', #14206 ) ;
#3915 = DIRECTION ( 'NONE',  ( 0.000000000000000000, 0.000000000000000000, -1.000000000000000000 ) ) ;
#3916 = CARTESIAN_POINT ( 'NONE',  ( -15.00000000000000355, 1.224646799147353454E-16, 0.000000000000000000 ) ) ;
#3917 = EDGE_CURVE ( 'NONE', #10979, #271, #13343, .T. ) ;
#3918 = DIRECTION ( 'NONE',  ( 1.000000000000000000, 0.000000000000000000, 0.000000000000000000 ) ) ;
#3919 = EDGE_CURVE ( 'NONE', #18537, #6978, #11105, .T. ) ;
#3920 = AXIS2_PLACEMENT_3D ( 'NONE', #7954, #14065, #16882 ) ;
#3921 = DIRECTION ( 'NONE',  ( 1.000000000000000000, 0.000000000000000000, 0.000000000000000000 ) ) ;
#3922 = ORIENTED_EDGE ( 'NONE', *, *, #13059, .T. ) ;
#3923 = CIRCLE ( 'NONE', #4565, 0.1999999999999987899 ) ;
#3924 = CARTESIAN_POINT ( 'NONE',  ( 1.749999999999998002, 12.96210679857786552, 24.89775460606837143 ) ) ;
#3925 = DIRECTION ( 'NONE',  ( -1.000000000000000000, -0.000000000000000000, -0.000000000000000000 ) ) ;
#3926 = ADVANCED_FACE ( 'NONE', ( #6380 ), #12512, .F. ) ;
#3927 = VERTEX_POINT ( 'NONE', #401 ) ;
#3928 = CIRCLE ( 'NONE', #5190, 4.200000000000000178 ) ;
#3929 = EDGE_CURVE ( 'NONE', #11356, #1421, #9718, .T. ) ;
#3930 = CARTESIAN_POINT ( 'NONE',  ( -17.28688694438836393, -7.664027248171298545, 35.00000000000000000 ) ) ;
#3931 = CARTESIAN_POINT ( 'NONE',  ( -3.499494075959840078, -3.499494075959791672, -14.34374999795161365 ) ) ;
#3932 = ORIENTED_EDGE ( 'NONE', *, *, #17857, .F. ) ;
#3933 = DIRECTION ( 'NONE',  ( 1.000000000000000000, 0.000000000000000000, 0.000000000000000000 ) ) ;
#3934 = CARTESIAN_POINT ( 'NONE',  ( 15.19790265903627358, 9.644882309621939598, -35.00000000000000000 ) ) ;
#3935 = FACE_BOUND ( 'NONE', #6753, .T. ) ;
#3936 = EDGE_LOOP ( 'NONE', ( #18370, #13354 ) ) ;
#3937 = EDGE_CURVE ( 'NONE', #4109, #3576, #7249, .T. ) ;
#3938 = CARTESIAN_POINT ( 'NONE',  ( 0.000000000000000000, 4.999999999999998224, 37.99999999999999289 ) ) ;
#3939 = VERTEX_POINT ( 'NONE', #7696 ) ;
#3940 = AXIS2_PLACEMENT_3D ( 'NONE', #3535, #17151, #4944 ) ;
#3941 = CONTEXT_DEPENDENT_SHAPE_REPRESENTATION ( #17919, #8434 ) ;
#3942 = SURFACE_STYLE_USAGE ( .BOTH. , #15859 ) ;
#3943 = LINE ( 'NONE', #15245, #5416 ) ;
#3944 = CIRCLE ( 'NONE', #5842, 1.000000000000004441 ) ;
#3945 = LINE ( 'NONE', #4045, #5469 ) ;
#3946 = ORIENTED_EDGE ( 'NONE', *, *, #4395, .F. ) ;
#3947 = CARTESIAN_POINT ( 'NONE',  ( 4.888101187500000222, -3.413342815706642518E-14, -6.468749997951615427 ) ) ;
#3948 = LINE ( 'NONE', #2149, #165 ) ;
#3949 = CARTESIAN_POINT ( 'NONE',  ( 0.000000000000000000, -8.936381166381891568E-14, 25.59481291497571220 ) ) ;
#3950 = ADVANCED_FACE ( 'NONE', ( #106 ), #18668, .F. ) ;
#3951 = ORIENTED_EDGE ( 'NONE', *, *, #18666, .F. ) ;
#3952 = PRESENTATION_LAYER_ASSIGNMENT (  '', '', ( #4264 ) ) ;
#3953 = DIRECTION ( 'NONE',  ( 1.000000000000000000, 0.000000000000000000, 0.000000000000000000 ) ) ;
#3954 = EDGE_CURVE ( 'NONE', #15369, #17299, #17816, .T. ) ;
#3955 = PRODUCT_DEFINITION_SHAPE ( 'NONE', 'NONE',  #19789 ) ;
#3956 = ORIENTED_EDGE ( 'NONE', *, *, #15296, .T. ) ;
#3957 = AXIS2_PLACEMENT_3D ( 'NONE', #2992, #3090, #9205 ) ;
#3958 = CARTESIAN_POINT ( 'NONE',  ( 6.656249997951614539, 4.936344801571308061, -2.849999999999989431 ) ) ;
#3959 = EDGE_CURVE ( 'NONE', #15013, #1448, #7142, .T. ) ;
#3960 = CARTESIAN_POINT ( 'NONE',  ( 0.000000000000000000, 0.000000000000000000, 5.700000000000001954 ) ) ;
#3961 = ORIENTED_EDGE ( 'NONE', *, *, #9048, .T. ) ;
#3962 = DIRECTION ( 'NONE',  ( 0.000000000000000000, 0.000000000000000000, 1.000000000000000000 ) ) ;
#3963 = COLOUR_RGB ( '', 0.40784314, 0.44705882, 0.49803922) ;
#3964 = TOROIDAL_SURFACE ( 'NONE', #19289, 7.800000000000000711, 0.1999999999999998723 ) ;
#3965 = SURFACE_SIDE_STYLE ('',( #14484 ) ) ;
#3966 = PRESENTATION_STYLE_ASSIGNMENT (( #2363 ) ) ;
#3967 = ORIENTED_EDGE ( 'NONE', *, *, #5488, .F. ) ;
#3968 = ORIENTED_EDGE ( 'NONE', *, *, #11443, .F. ) ;
#3969 = CARTESIAN_POINT ( 'NONE',  ( -12.32184790671639085, 13.12143529358541549, 32.00000000000000000 ) ) ;
#3970 = ADVANCED_FACE ( 'NONE', ( #8663 ), #11968, .F. ) ;
#3971 = ADVANCED_FACE ( 'NONE', ( #14681 ), #8870, .F. ) ;
#3972 = AXIS2_PLACEMENT_3D ( 'NONE', #15953, #6160, #12279 ) ;
#3973 = DIRECTION ( 'NONE',  ( -1.000000000000000000, -0.000000000000000000, -0.000000000000000000 ) ) ;
#3974 = CARTESIAN_POINT ( 'NONE',  ( 1.039999999999996483, -12.96210679857803783, 24.89775460606827551 ) ) ;
#3975 = ORIENTED_EDGE ( 'NONE', *, *, #5358, .F. ) ;
#3976 = CARTESIAN_POINT ( 'NONE',  ( -17.11901729331276911, 5.562305898749051458, -35.00000000000000000 ) ) ;
#3977 = VECTOR ( 'NONE', #9960, 1000.000000000000000 ) ;
#3978 = ORIENTED_EDGE ( 'NONE', *, *, #10697, .T. ) ;
#3979 = CARTESIAN_POINT ( 'NONE',  ( 0.000000000000000000, 0.000000000000000000, 0.000000000000000000 ) ) ;
#3980 = CIRCLE ( 'NONE', #17723, 4.200000000000000178 ) ;
#3981 = CARTESIAN_POINT ( 'NONE',  ( -41.99999999999999289, -3.184081677783117402E-15, 0.000000000000000000 ) ) ;
#3982 = EDGE_CURVE ( 'NONE', #9010, #11813, #1834, .T. ) ;
#3983 = CARTESIAN_POINT ( 'NONE',  ( 1.039999999999997815, 27.68468304288265003, -4.633866840648637186 ) ) ;
#3984 = DIRECTION ( 'NONE',  ( 0.000000000000000000, 0.000000000000000000, -1.000000000000000000 ) ) ;
#3985 = DIRECTION ( 'NONE',  ( -1.000000000000000000, -0.000000000000000000, -0.000000000000000000 ) ) ;
#3986 =( NAMED_UNIT ( * ) SI_UNIT ( $, .STERADIAN. ) SOLID_ANGLE_UNIT ( ) );
#3987 = DIRECTION ( 'NONE',  ( 0.000000000000000000, 0.000000000000000000, 1.000000000000000000 ) ) ;
#3988 = VERTEX_POINT ( 'NONE', #14970 ) ;
#3989 = DIRECTION ( 'NONE',  ( 0.000000000000000000, 0.000000000000000000, 1.000000000000000000 ) ) ;
#3990 = AXIS2_PLACEMENT_3D ( 'NONE', #14854, #2635, #1151 ) ;
#3991 = CYLINDRICAL_SURFACE ( 'NONE', #5207, 5.400000000000000355 ) ;
#3992 = UNCERTAINTY_MEASURE_WITH_UNIT (LENGTH_MEASURE( 1.000000000000000082E-05 ), #19051, 'distance_accuracy_value', 'NONE');
#3993 = CARTESIAN_POINT ( 'NONE',  ( 4.780397808154266848, 1.280903732194421218, -9.343749997951615427 ) ) ;
#3994 = EDGE_CURVE ( 'NONE', #19037, #2313, #5241, .T. ) ;
#3995 = CARTESIAN_POINT ( 'NONE',  ( 3.293609449816393475, -7.263869220928335757, -0.01675691374233746408 ) ) ;
#3996 = CARTESIAN_POINT ( 'NONE',  ( 2.030753616560878161, -12.05220173035456632, 24.80264696524878687 ) ) ;
#3997 = VERTEX_POINT ( 'NONE', #5557 ) ;
#3998 = CARTESIAN_POINT ( 'NONE',  ( -12.86923836996420611, -11.47363181547641275, 32.00000000000000000 ) ) ;
#3999 = LINE ( 'NONE', #16303, #15549 ) ;
#4000 = EDGE_LOOP ( 'NONE', ( #9435, #9994 ) ) ;
#4001 = SURFACE_STYLE_USAGE ( .BOTH. , #16012 ) ;
#4002 = EDGE_CURVE ( 'NONE', #18335, #10204, #17773, .T. ) ;
#4003 = DIRECTION ( 'NONE',  ( 1.000000000000000000, 0.000000000000000000, 0.000000000000000000 ) ) ;
#4004 = AXIS2_PLACEMENT_3D ( 'NONE', #16285, #11677, #8778 ) ;
#4005 = VECTOR ( 'NONE', #7765, 1000.000000000000000 ) ;
#4006 = DIRECTION ( 'NONE',  ( 0.000000000000000000, 0.000000000000000000, 1.000000000000000000 ) ) ;
#4007 = CARTESIAN_POINT ( 'NONE',  ( 2.789999999999999147, 22.25075486061738772, 9.324097380959527115 ) ) ;
#4008 = ORIENTED_EDGE ( 'NONE', *, *, #14952, .T. ) ;
#4009 = CYLINDRICAL_SURFACE ( 'NONE', #5615, 3.000000000000000000 ) ;
#4010 =( NAMED_UNIT ( * ) PLANE_ANGLE_UNIT ( ) SI_UNIT ( $, .RADIAN. ) );
#4011 = DIRECTION ( 'NONE',  ( 0.000000000000000000, 0.000000000000000000, 1.000000000000000000 ) ) ;
#4012 = ORIENTED_EDGE ( 'NONE', *, *, #18752, .T. ) ;
#4013 = CARTESIAN_POINT ( 'NONE',  ( 11.31249999590322375, -4.235925505221111997, -3.814044456245531567 ) ) ;
#4014 = ORIENTED_EDGE ( 'NONE', *, *, #10919, .T. ) ;
#4015 = CARTESIAN_POINT ( 'NONE',  ( -13.32184790671639618, 13.12143529358541549, -32.00000000000000000 ) ) ;
#4016 = ADVANCED_FACE ( 'NONE', ( #17871 ), #18786, .T. ) ;
#4017 = CARTESIAN_POINT ( 'NONE',  ( -5.421022142882375938, 1.761396867937200517, -8.312499995903225525 ) ) ;
#4018 = DIRECTION ( 'NONE',  ( 1.000000000000000000, -0.000000000000000000, -0.000000000000000000 ) ) ;
#4019 = CIRCLE ( 'NONE', #10097, 7.937500000000000000 ) ;
#4020 = DIRECTION ( 'NONE',  ( 1.000000000000000000, 0.000000000000000000, 0.000000000000000000 ) ) ;
#4021 = AXIS2_PLACEMENT_3D ( 'NONE', #15172, #12836, #3435 ) ;
#4022 = EDGE_LOOP ( 'NONE', ( #17706, #2141, #14777, #12014 ) ) ;
#4023 = FACE_BOUND ( 'NONE', #17376, .T. ) ;
#4024 = CYLINDRICAL_SURFACE ( 'NONE', #3706, 1.000000000000000888 ) ;
#4025 = EDGE_LOOP ( 'NONE', ( #11265, #15956, #13762, #7318 ) ) ;
#4026 = EDGE_CURVE ( 'NONE', #13429, #540, #19091, .T. ) ;
#4027 = DIRECTION ( 'NONE',  ( -1.000000000000000000, 0.000000000000000000, -0.000000000000000000 ) ) ;
#4028 = EDGE_CURVE ( 'NONE', #3750, #1726, #9854, .T. ) ;
#4029 = DIRECTION ( 'NONE',  ( -1.000000000000000000, -0.000000000000000000, -0.000000000000000000 ) ) ;
#4030 = EDGE_CURVE ( 'NONE', #3614, #4548, #18561, .T. ) ;
#4031 = ORIENTED_EDGE ( 'NONE', *, *, #13132, .T. ) ;
#4032 = AXIS2_PLACEMENT_3D ( 'NONE', #18818, #821, #2207 ) ;
#4033 = CYLINDRICAL_SURFACE ( 'NONE', #14237, 10.00000000000000000 ) ;
#4034 = CARTESIAN_POINT ( 'NONE',  ( -5.000000000000000000, -2.000000000000001332, 37.99999999999999289 ) ) ;
#4035 = FACE_BOUND ( 'NONE', #9481, .T. ) ;
#4036 = AXIS2_PLACEMENT_3D ( 'NONE', #14828, #7100, #16327 ) ;
#4037 = VERTEX_POINT ( 'NONE', #5951 ) ;
#4038 = CARTESIAN_POINT ( 'NONE',  ( -17.11901729331276911, 5.562305898749051458, 35.00000000000000000 ) ) ;
#4039 = FACE_OUTER_BOUND ( 'NONE', #14358, .T. ) ;
#4040 = ORIENTED_EDGE ( 'NONE', *, *, #12523, .F. ) ;
#4041 = FACE_OUTER_BOUND ( 'NONE', #1306, .T. ) ;
#4042 = DIRECTION ( 'NONE',  ( 0.000000000000000000, 0.000000000000000000, -1.000000000000000000 ) ) ;
#4043 = EDGE_CURVE ( 'NONE', #9272, #13507, #917, .T. ) ;
#4044 = EDGE_CURVE ( 'NONE', #11866, #18865, #3065, .T. ) ;
#4045 = CARTESIAN_POINT ( 'NONE',  ( -5.207209108562805611, 2.318398865532109276, 0.000000000000000000 ) ) ;
#4046 = EDGE_LOOP ( 'NONE', ( #10611, #14688, #10267, #6336 ) ) ;
#4047 = DIRECTION ( 'NONE',  ( 0.000000000000000000, -1.000000000000000000, 0.000000000000000000 ) ) ;
#4048 = CARTESIAN_POINT ( 'NONE',  ( 8.500000000000005329, 1.493657965219485018, 5.574407415329170057 ) ) ;
#4049 = CARTESIAN_POINT ( 'NONE',  ( -16.19790265903627713, 9.644882309621941374, -32.00000000000000000 ) ) ;
#4050 = ORIENTED_EDGE ( 'NONE', *, *, #12191, .F. ) ;
#4051 = B_SPLINE_CURVE_WITH_KNOTS ( 'NONE', 3,
 ( #12143, #2921, #10541, #132, #4432, #10740 ),
 .UNSPECIFIED., .F., .F.,
 ( 4, 2, 4 ),
 ( 0.0004963285629697519611, 0.002127826186449857486, 0.003759323809929962686 ),
 .UNSPECIFIED. ) ;
#4052 = AXIS2_PLACEMENT_3D ( 'NONE', #1406, #12008, #5593 ) ;
#4053 = AXIS2_PLACEMENT_3D ( 'NONE', #12912, #13792, #88 ) ;
#4054 = CARTESIAN_POINT ( 'NONE',  ( 2.765633920072236407, -2.336989772644440855, 24.63872515616082026 ) ) ;
#4055 = ORIENTED_EDGE ( 'NONE', *, *, #2952, .F. ) ;
#4056 = CARTESIAN_POINT ( 'NONE',  ( 7.078124996927420476, -4.584782303107560963, -2.647025296875054057 ) ) ;
#4057 = CARTESIAN_POINT ( 'NONE',  ( 7.312499995903225525, -4.936344801571327601, 2.849999999999954348 ) ) ;
#4058 = ORIENTED_EDGE ( 'NONE', *, *, #19726, .F. ) ;
#4059 = CARTESIAN_POINT ( 'NONE',  ( -0.5109457054261112852, 4.861323657744413218, -14.46874999795161720 ) ) ;
#4060 = CIRCLE ( 'NONE', #5958, 28.06981291497571362 ) ;
#4061 = AXIS2_PLACEMENT_3D ( 'NONE', #13938, #4828, #10935 ) ;
#4062 = ADVANCED_FACE ( 'NONE', ( #351 ), #1204, .T. ) ;
#4063 = ORIENTED_EDGE ( 'NONE', *, *, #9147, .F. ) ;
#4064 = EDGE_LOOP ( 'NONE', ( #4674, #4076 ) ) ;
#4065 = EDGE_CURVE ( 'NONE', #18486, #4381, #15735, .T. ) ;
#4066 = DIRECTION ( 'NONE',  ( 0.000000000000000000, 0.000000000000000000, -1.000000000000000000 ) ) ;
#4067 = CARTESIAN_POINT ( 'NONE',  ( 1.394999999999999574, -4.147968289691484678, 27.76164181293050603 ) ) ;
#4068 = ORIENTED_EDGE ( 'NONE', *, *, #13316, .T. ) ;
#4069 = CIRCLE ( 'NONE', #2800, 1.000000000000002665 ) ;
#4070 = DIRECTION ( 'NONE',  ( 0.000000000000000000, 0.000000000000000000, 1.000000000000000000 ) ) ;
#4071 = VERTEX_POINT ( 'NONE', #10965 ) ;
#4072 = CARTESIAN_POINT ( 'NONE',  ( 111.3234999999999957, 4.898587196589412829E-16, -4.000000000000000000 ) ) ;
#4073 = EDGE_CURVE ( 'NONE', #2268, #6765, #18757, .T. ) ;
#4074 = CARTESIAN_POINT ( 'NONE',  ( 7.343749997951615427, -3.846120219227900705, -3.114526743279308896 ) ) ;
#4075 = VECTOR ( 'NONE', #15411, 1000.000000000000000 ) ;
#4076 = ORIENTED_EDGE ( 'NONE', *, *, #14792, .F. ) ;
#4077 = CARTESIAN_POINT ( 'NONE',  ( -2.000000000000001776, 0.000000000000000000, 0.000000000000000000 ) ) ;
#4078 = AXIS2_PLACEMENT_3D ( 'NONE', #17849, #4144, #10256 ) ;
#4079 = EDGE_CURVE ( 'NONE', #12768, #6633, #235, .T. ) ;
#4080 = ADVANCED_FACE ( 'NONE', ( #18858, #17261 ), #15663, .T. ) ;
#4081 = DIRECTION ( 'NONE',  ( 1.000000000000000000, 0.000000000000000000, 0.000000000000000000 ) ) ;
#4082 = CARTESIAN_POINT ( 'NONE',  ( 2.789999999999999147, 18.28042085475301093, -15.74360496233361673 ) ) ;
#4083 = CARTESIAN_POINT ( 'NONE',  ( 8.343749997951613651, -4.942249507334558700, 0.2590123213420630899 ) ) ;
#4084 = B_SPLINE_CURVE_WITH_KNOTS ( 'NONE', 3,
 ( #10340, #19041, #10050, #13237, #1127, #5613 ),
 .UNSPECIFIED., .F., .F.,
 ( 4, 2, 4 ),
 ( 4.462636808902389156E-07, 0.001879885123572227514, 0.003759323983463565104 ),
 .UNSPECIFIED. ) ;
#4085 = DIRECTION ( 'NONE',  ( 0.000000000000000000, 0.000000000000000000, 1.000000000000000000 ) ) ;
#4086 = SURFACE_SIDE_STYLE ('',( #981 ) ) ;
#4087 = CARTESIAN_POINT ( 'NONE',  ( 1.749999999999998002, -24.89775460606842117, 12.96210679857777137 ) ) ;
#4088 = VERTEX_POINT ( 'NONE', #3754 ) ;
#4089 = LINE ( 'NONE', #13480, #12079 ) ;
#4090 = AXIS2_PLACEMENT_3D ( 'NONE', #10493, #17892, #11987 ) ;
#4091 = CARTESIAN_POINT ( 'NONE',  ( 8.671566133830875600, 15.77352024078954784, -32.00000000000000000 ) ) ;
#4092 = CARTESIAN_POINT ( 'NONE',  ( -5.575441324182679459, 1.185096637661293251, -10.00000000000000533 ) ) ;
#4093 = VECTOR ( 'NONE', #9042, 1000.000000000000000 ) ;
#4094 = CARTESIAN_POINT ( 'NONE',  ( 1.280903732194421440, -4.780397808154265071, -13.96874999795161365 ) ) ;
#4095 = CARTESIAN_POINT ( 'NONE',  ( 7.671566133830872047, 15.77352024078954784, 35.00000000000000000 ) ) ;
#4096 = ORIENTED_EDGE ( 'NONE', *, *, #6801, .T. ) ;
#4097 = CARTESIAN_POINT ( 'NONE',  ( 1.394999999999999574, 12.52377138324224148, 25.12109765559658570 ) ) ;
#4098 = CARTESIAN_POINT ( 'NONE',  ( 0.000000000000000000, -7.909232158574647009, -24.34211360614308006 ) ) ;
#4099 = ORIENTED_EDGE ( 'NONE', *, *, #5407, .T. ) ;
#4100 = DIRECTION ( 'NONE',  ( 1.000000000000000000, 0.000000000000000000, 0.000000000000000000 ) ) ;
#4101 = CARTESIAN_POINT ( 'NONE',  ( 2.765633920072234631, 5.391175441198615914, 24.15498966839965078 ) ) ;
#4102 = VECTOR ( 'NONE', #14075, 1000.000000000000000 ) ;
#4103 = CARTESIAN_POINT ( 'NONE',  ( 2.783068930044319433, -18.43696893154769612, 16.17493693894872564 ) ) ;
#4104 = DIRECTION ( 'NONE',  ( 1.000000000000000000, 0.000000000000000000, 0.000000000000000000 ) ) ;
#4105 = ORIENTED_EDGE ( 'NONE', *, *, #14586, .T. ) ;
#4106 = DIRECTION ( 'NONE',  ( 1.000000000000000000, 0.000000000000000000, 0.000000000000000000 ) ) ;
#4107 = DIRECTION ( 'NONE',  ( 0.000000000000000000, 0.000000000000000000, 1.000000000000000000 ) ) ;
#4108 = CARTESIAN_POINT ( 'NONE',  ( 0.006974693931642885793, -18.43727551351043203, 16.17543236987982525 ) ) ;
#4109 = VERTEX_POINT ( 'NONE', #7947 ) ;
#4110 = DIRECTION ( 'NONE',  ( 0.000000000000000000, 0.000000000000000000, 1.000000000000000000 ) ) ;
#4111 = EDGE_LOOP ( 'NONE', ( #14738, #10440, #8129, #19034 ) ) ;
#4112 = CARTESIAN_POINT ( 'NONE',  ( 0.000000000000000000, 20.62201879784911540, 12.52067188844362100 ) ) ;
#4113 = CARTESIAN_POINT ( 'NONE',  ( -18.68117051311639543, -3.372863662543042818, 32.00000000000000000 ) ) ;
#4114 = PRODUCT ( 'angular contact ball bearing_68_iso_ISO 15 ABB - 188 - 12,SI,NC,12_68', 'angular contact ball bearing_68_iso_ISO 15 ABB - 188 - 12,SI,NC,12_68', '', ( #15657 ) ) ;
#4115 = CARTESIAN_POINT ( 'NONE',  ( 2.000000000000001776, 0.000000000000000000, 0.000000000000000000 ) ) ;
#4116 = AXIS2_PLACEMENT_3D ( 'NONE', #15043, #1042, #1332 ) ;
#4117 = CARTESIAN_POINT ( 'NONE',  ( -0.9027913098498572264, 5.700000000000000178, -10.50000000000000533 ) ) ;
#4118 = EDGE_LOOP ( 'NONE', ( #6163, #19732, #11072, #4810, #13734 ) ) ;
#4119 = CARTESIAN_POINT ( 'NONE',  ( 2.444050593749960587, -4.233219804643904460, -6.468749997951615427 ) ) ;
#4120 = CARTESIAN_POINT ( 'NONE',  ( 5.700000000000001066, -3.980288726281172656E-14, -6.656249997951614539 ) ) ;
#4121 = VERTEX_POINT ( 'NONE', #6434 ) ;
#4122 = ORIENTED_EDGE ( 'NONE', *, *, #8103, .T. ) ;
#4123 =( BOUNDED_CURVE ( )  B_SPLINE_CURVE ( 2, ( #18534, #12438, #17139, #10837, #13839, #15638, #1536, #9443, #9241 ),
 .UNSPECIFIED., .F., .F. ) 
 B_SPLINE_CURVE_WITH_KNOTS ( ( 3, 2, 2, 2, 3 ),
 ( 0.000000000000000000, 0.05000000000000000278, 0.1000000000000000056, 0.1499999999999999944, 0.1666819079834106210 ),
 .UNSPECIFIED. ) 
 CURVE ( )  GEOMETRIC_REPRESENTATION_ITEM ( )  RATIONAL_B_SPLINE_CURVE ( ( 1.000000000000000000, 0.9876883405951377704, 1.000000000000000000, 0.9876883405951377704, 1.000000000000000000, 0.9876883405951377704, 1.000000000000000000, 0.9958923606136999007, 0.9945256517182514688 ) ) 
 REPRESENTATION_ITEM ( '' )  );
#4124 = ADVANCED_FACE ( 'NONE', ( #19057 ), #11259, .F. ) ;
#4125 = CARTESIAN_POINT ( 'NONE',  ( -3.255998204157480203, -17.85806462366060288, 32.00000000000000000 ) ) ;
#4126 = CARTESIAN_POINT ( 'NONE',  ( 0.9027913098498173694, -5.700000000000005507, -11.81249999590322552 ) ) ;
#4127 = VECTOR ( 'NONE', #9882, 1000.000000000000000 ) ;
#4128 = ORIENTED_EDGE ( 'NONE', *, *, #11166, .F. ) ;
#4129 = CARTESIAN_POINT ( 'NONE',  ( 9.000000000000001776, 1.102182119232617911E-15, -30.00000000000000355 ) ) ;
#4130 = FACE_OUTER_BOUND ( 'NONE', #652, .T. ) ;
#4131 = CARTESIAN_POINT ( 'NONE',  ( 12.92161831991541554, -3.713244971082748425, 3.181176262573032432 ) ) ;
#4132 = EDGE_LOOP ( 'NONE', ( #18424, #16136, #12230, #12543 ) ) ;
#4133 = DIRECTION ( 'NONE',  ( -1.000000000000000000, 0.000000000000000000, 0.000000000000000000 ) ) ;
#4134 = ORIENTED_EDGE ( 'NONE', *, *, #17837, .T. ) ;
#4135 = CARTESIAN_POINT ( 'NONE',  ( 91.50000000000000000, 0.000000000000000000, 0.000000000000000000 ) ) ;
#4136 = ORIENTED_EDGE ( 'NONE', *, *, #15282, .F. ) ;
#4137 = AXIS2_PLACEMENT_3D ( 'NONE', #4457, #6237, #10566 ) ;
#4138 = CARTESIAN_POINT ( 'NONE',  ( 6.968749997951614539, 3.846120219227923798, 3.114526743279282694 ) ) ;
#4139 = FILL_AREA_STYLE ('',( #3193 ) ) ;
#4140 = CYLINDRICAL_SURFACE ( 'NONE', #10213, 1.000000000000002665 ) ;
#4141 = DIRECTION ( 'NONE',  ( 1.000000000000000000, 0.000000000000000000, 0.000000000000000000 ) ) ;
#4142 = CARTESIAN_POINT ( 'NONE',  ( -36.00000000000000000, -2.311115933264683024E-31, 0.000000000000000000 ) ) ;
#4143 = CARTESIAN_POINT ( 'NONE',  ( 0.000000000000000000, 0.000000000000000000, 0.000000000000000000 ) ) ;
#4144 = DIRECTION ( 'NONE',  ( 1.000000000000000000, 6.419766481290786633E-33, -0.000000000000000000 ) ) ;
#4145 = ORIENTED_EDGE ( 'NONE', *, *, #11453, .F. ) ;
#4146 = ADVANCED_FACE ( 'NONE', ( #9470 ), #15767, .F. ) ;
#4147 = CARTESIAN_POINT ( 'NONE',  ( 0.5279273746168620107, 4.996265754456365116, 26.57710921259763026 ) ) ;
#4148 = AXIS2_PLACEMENT_3D ( 'NONE', #11229, #18725, #15834 ) ;
#4149 = VERTEX_POINT ( 'NONE', #9775 ) ;
#4150 = EDGE_CURVE ( 'NONE', #11541, #11454, #9876, .T. ) ;
#4151 = DIRECTION ( 'NONE',  ( 0.000000000000000000, 0.000000000000000000, 1.000000000000000000 ) ) ;
#4152 = CARTESIAN_POINT ( 'NONE',  ( 5.626241948324195441, -16.73597674598852691, -32.00000000000000000 ) ) ;
#4153 = CYLINDRICAL_SURFACE ( 'NONE', #1262, 4.500000000000000000 ) ;
#4154 = DIRECTION ( 'NONE',  ( 0.000000000000000000, 0.000000000000000000, 1.000000000000000000 ) ) ;
#4155 = EDGE_LOOP ( 'NONE', ( #13488, #15124, #11388, #6997, #13579, #15531, #13777 ) ) ;
#4156 = CARTESIAN_POINT ( 'NONE',  ( -4.861323657744413218, -0.5109457054261099529, -9.843749997951615427 ) ) ;
#4157 = CARTESIAN_POINT ( 'NONE',  ( 0.000000000000000000, 0.000000000000000000, 38.00000000000000711 ) ) ;
#4158 = CARTESIAN_POINT ( 'NONE',  ( 2.318398865532074193, 5.207209108562820710, -9.000000000000005329 ) ) ;
#4159 = ORIENTED_EDGE ( 'NONE', *, *, #13395, .T. ) ;
#4160 = VERTEX_POINT ( 'NONE', #9668 ) ;
#4161 = CARTESIAN_POINT ( 'NONE',  ( 0.000000000000000000, 12.52067188844351442, 20.62201879784919001 ) ) ;
#4162 = TOROIDAL_SURFACE ( 'NONE', #1607, 4.200000000000000178, 0.1999999999999998723 ) ;
#4163 = AXIS2_PLACEMENT_3D ( 'NONE', #18528, #8011, #1727 ) ;
#4164 = ORIENTED_EDGE ( 'NONE', *, *, #124, .T. ) ;
#4165 = EDGE_CURVE ( 'NONE', #12173, #13180, #2050, .T. ) ;
#4166 = CARTESIAN_POINT ( 'NONE',  ( 0.5279273746168618997, -26.57710921259763737, 4.996265754456265640 ) ) ;
#4167 = ORIENTED_EDGE ( 'NONE', *, *, #237, .T. ) ;
#4168 = CARTESIAN_POINT ( 'NONE',  ( -8.000000000000000000, 0.000000000000000000, -33.00000000000000000 ) ) ;
#4169 = DIRECTION ( 'NONE',  ( 0.000000000000000000, 0.000000000000000000, 1.000000000000000000 ) ) ;
#4170 = EDGE_CURVE ( 'NONE', #11710, #8006, #14627, .T. ) ;
#4171 = ORIENTED_EDGE ( 'NONE', *, *, #11692, .T. ) ;
#4172 = CARTESIAN_POINT ( 'NONE',  ( 11.06250000000000000, 0.000000000000000000, 0.000000000000000000 ) ) ;
#4173 = B_SPLINE_CURVE_WITH_KNOTS ( 'NONE', 3,
 ( #19609, #4108, #18215, #2596 ),
 .UNSPECIFIED., .F., .F.,
 ( 4, 4 ),
 ( 2.324263106244687463E-07, 0.0006888201370294697295 ),
 .UNSPECIFIED. ) ;
#4174 = EDGE_CURVE ( 'NONE', #12336, #4629, #3456, .T. ) ;
#4175 = VECTOR ( 'NONE', #5077, 1000.000000000000000 ) ;
#4176 = PRESENTATION_LAYER_ASSIGNMENT (  '', '', ( #9616 ) ) ;
#4177 = PLANE ( 'NONE',  #13191 ) ;
#4178 = FACE_OUTER_BOUND ( 'NONE', #1548, .T. ) ;
#4179 = CARTESIAN_POINT ( 'NONE',  ( 12.34374999795161543, 1.773574444220725743, 4.620319390059829168 ) ) ;
#4180 = CARTESIAN_POINT ( 'NONE',  ( 0.000000000000000000, 7.347880794884119736E-16, -6.000000000000000000 ) ) ;
#4181 = CARTESIAN_POINT ( 'NONE',  ( 2.783068930044318545, 16.17493693894878604, 18.43696893154764282 ) ) ;
#4182 = ORIENTED_EDGE ( 'NONE', *, *, #333, .F. ) ;
#4183 = EDGE_CURVE ( 'NONE', #768, #3194, #9515, .T. ) ;
#4184 = CARTESIAN_POINT ( 'NONE',  ( 4.762500000000000178, 0.000000000000000000, -25.03750572909317285 ) ) ;
#4185 = DIRECTION ( 'NONE',  ( 1.000000000000000000, 0.000000000000000000, 0.000000000000000000 ) ) ;
#4186 = UNCERTAINTY_MEASURE_WITH_UNIT (LENGTH_MEASURE( 1.000000000000000082E-05 ), #14912, 'distance_accuracy_value', 'NONE');
#4187 = CARTESIAN_POINT ( 'NONE',  ( 2.000000000000000000, -2.000000000000001776, 37.99999999999999289 ) ) ;
#4188 = DIRECTION ( 'NONE',  ( 0.000000000000000000, 0.000000000000000000, -1.000000000000000000 ) ) ;
#4189 = VECTOR ( 'NONE', #10654, 1000.000000000000000 ) ;
#4190 = CARTESIAN_POINT ( 'NONE',  ( 12.99999999999999467, 4.416988234087969367, 2.093740232017179181 ) ) ;
#4191 = EDGE_CURVE ( 'NONE', #18200, #5529, #14946, .T. ) ;
#4192 = ORIENTED_EDGE ( 'NONE', *, *, #9827, .F. ) ;
#4193 = ADVANCED_FACE ( 'NONE', ( #13256 ), #19342, .T. ) ;
#4194 = CARTESIAN_POINT ( 'NONE',  ( -2.500000000000002220, 0.000000000000000000, -8.073750000000021743 ) ) ;
#4195 = CARTESIAN_POINT ( 'NONE',  ( 11.58013454126452579, -14.56230589874905412, 32.00000000000000000 ) ) ;
#4196 = ORIENTED_EDGE ( 'NONE', *, *, #9722, .F. ) ;
#4197 = CARTESIAN_POINT ( 'NONE',  ( 9.312499995903225525, 2.318398865532038666, 5.207209108562838473 ) ) ;
#4198 = CARTESIAN_POINT ( 'NONE',  ( 10.81249999590322375, -4.840010801796461593, -3.143139765844656708 ) ) ;
#4199 = EDGE_CURVE ( 'NONE', #813, #6746, #6935, .T. ) ;
#4200 = LINE ( 'NONE', #718, #2936 ) ;
#4201 = CARTESIAN_POINT ( 'NONE',  ( 2.789999999999999147, 24.63872515616082737, -2.336989772644355590 ) ) ;
#4202 = ORIENTED_EDGE ( 'NONE', *, *, #3779, .T. ) ;
#4203 = CARTESIAN_POINT ( 'NONE',  ( 2.789999999999999147, -2.336989772644097574, -24.63872515616085224 ) ) ;
#4204 = CARTESIAN_POINT ( 'NONE',  ( 4.781284448697187273, -1.016293382781444654, -10.84374999795161543 ) ) ;
#4205 = EDGE_CURVE ( 'NONE', #5161, #4088, #15908, .T. ) ;
#4206 = AXIS2_PLACEMENT_3D ( 'NONE', #15959, #5628, #14461 ) ;
#4207 = CARTESIAN_POINT ( 'NONE',  ( 13.00000000000000533, -4.611396867937178179, -3.350375938067128967 ) ) ;
#4208 = ORIENTED_EDGE ( 'NONE', *, *, #660, .T. ) ;
#4209 = CARTESIAN_POINT ( 'NONE',  ( -13.86923836996420967, -11.47363181547641275, 35.00000000000000000 ) ) ;
#4210 = VERTEX_POINT ( 'NONE', #4049 ) ;
#4211 = CARTESIAN_POINT ( 'NONE',  ( 9.968749997951615427, -4.409619785863921670, 2.246813503491803310 ) ) ;
#4212 = CARTESIAN_POINT ( 'NONE',  ( 0.000000000000000000, 5.535312321043032391, -23.48180575137725867 ) ) ;
#4213 = CARTESIAN_POINT ( 'NONE',  ( -90.00000000000000000, 0.000000000000000000, 0.000000000000000000 ) ) ;
#4214 = EDGE_CURVE ( 'NONE', #881, #16591, #18456, .T. ) ;
#4215 = DIRECTION ( 'NONE',  ( 0.000000000000000000, 0.000000000000000000, 1.000000000000000000 ) ) ;
#4216 = ORIENTED_EDGE ( 'NONE', *, *, #14169, .T. ) ;
#4217 = CARTESIAN_POINT ( 'NONE',  ( -1.988169868018624609, -4.465502636338009701, -9.843749997951615427 ) ) ;
#4218 = DIRECTION ( 'NONE',  ( 0.000000000000000000, 0.000000000000000000, -1.000000000000000000 ) ) ;
#4219 = AXIS2_PLACEMENT_3D ( 'NONE', #1497, #13397, #10703 ) ;
#4220 = VERTEX_POINT ( 'NONE', #16063 ) ;
#4221 = CIRCLE ( 'NONE', #716, 1.000000000000000888 ) ;
#4222 = AXIS2_PLACEMENT_3D ( 'NONE', #18702, #2192, #16112 ) ;
#4223 = AXIS2_PLACEMENT_3D ( 'NONE', #12998, #8290, #16292 ) ;
#4224 = DIRECTION ( 'NONE',  ( 1.000000000000000000, 0.000000000000000000, 0.000000000000000000 ) ) ;
#4225 = DIRECTION ( 'NONE',  ( -1.000000000000000000, -0.000000000000000000, -0.000000000000000000 ) ) ;
#4226 = ORIENTED_EDGE ( 'NONE', *, *, #15830, .F. ) ;
#4227 = CARTESIAN_POINT ( 'NONE',  ( 13.00000000000000000, 4.125339889944109828, -2.622041954598519187 ) ) ;
#4228 = CYLINDRICAL_SURFACE ( 'NONE', #5317, 9.000000000000000000 ) ;
#4229 = FACE_BOUND ( 'NONE', #11750, .T. ) ;
#4230 = ORIENTED_EDGE ( 'NONE', *, *, #14483, .T. ) ;
#4231 = CARTESIAN_POINT ( 'NONE',  ( 1.899999999999999023, 0.000000000000000000, -6.760799999999997034 ) ) ;
#4232 = VERTEX_POINT ( 'NONE', #14661 ) ;
#4233 = ADVANCED_BREP_SHAPE_REPRESENTATION ( '', ( #9431, #16724 ), #16113 ) ;
#4234 = CARTESIAN_POINT ( 'NONE',  ( 0.1855656748306439008, -25.77772010606603814, -2.851997810081915663 ) ) ;
#4235 = AXIS2_PLACEMENT_3D ( 'NONE', #16684, #13471, #6058 ) ;
#4236 = VERTEX_POINT ( 'NONE', #10157 ) ;
#4237 = CIRCLE ( 'NONE', #15425, 1.000000000000004441 ) ;
#4238 =( NAMED_UNIT ( * ) PLANE_ANGLE_UNIT ( ) SI_UNIT ( $, .RADIAN. ) );
#4239 = CYLINDRICAL_SURFACE ( 'NONE', #8995, 1.000000000000004441 ) ;
#4240 = CARTESIAN_POINT ( 'NONE',  ( -19.00000000000000355, 1.224646799147353207E-16, 0.000000000000000000 ) ) ;
#4241 = CARTESIAN_POINT ( 'NONE',  ( -90.00000000000000000, 0.000000000000000000, -8.265000000000021885 ) ) ;
#4242 = CARTESIAN_POINT ( 'NONE',  ( 16.28688694438835327, -7.664027248171309203, -35.00000000000000000 ) ) ;
#4243 = EDGE_CURVE ( 'NONE', #8143, #4160, #7575, .T. ) ;
#4244 = VERTEX_POINT ( 'NONE', #1146 ) ;
#4245 = PRESENTATION_LAYER_ASSIGNMENT (  '', '', ( #414 ) ) ;
#4246 =( BOUNDED_CURVE ( )  B_SPLINE_CURVE ( 2, ( #14163, #9673, #5253, #8047, #12863, #18661, #2053, #14266, #17265, #2154, #8259, #3551, #354, #3853, #11369, #15771, #15667 ),
 .UNSPECIFIED., .F., .F. ) 
 B_SPLINE_CURVE_WITH_KNOTS ( ( 3, 2, 2, 2, 2, 2, 2, 2, 3 ),
 ( 0.000000000000000000, 0.05000000000000000971, 0.1000000000000000194, 0.1499999999999999944, 0.2000000000000000389, 0.2500000000000000000, 0.2999999999999999889, 0.3499999999999999223, 0.4000000000000000777 ),
 .UNSPECIFIED. ) 
 CURVE ( )  GEOMETRIC_REPRESENTATION_ITEM ( )  RATIONAL_B_SPLINE_CURVE ( ( 1.000000000000000000, 0.9876883405951377704, 1.000000000000000000, 0.9876883405951377704, 1.000000000000000000, 0.9876883405951377704, 1.000000000000000000, 0.9876883405951377704, 1.000000000000000000, 0.9876883405951377704, 1.000000000000000000, 0.9876883405951377704, 1.000000000000000000, 0.9876883405951377704, 1.000000000000000000, 0.9876883405951377704, 1.000000000000000000 ) ) 
 REPRESENTATION_ITEM ( '' )  );
#4247 = CARTESIAN_POINT ( 'NONE',  ( 2.000000000000001776, 0.000000000000000000, -6.735000000000022524 ) ) ;
#4248 = AXIS2_PLACEMENT_3D ( 'NONE', #6038, #12159, #7134 ) ;
#4249 = ORIENTED_EDGE ( 'NONE', *, *, #744, .F. ) ;
#4250 = ADVANCED_FACE ( 'NONE', ( #2534 ), #5347, .F. ) ;
#4251 = FACE_OUTER_BOUND ( 'NONE', #17462, .T. ) ;
#4252 = CIRCLE ( 'NONE', #11906, 24.12539914357697413 ) ;
#4253 = CARTESIAN_POINT ( 'NONE',  ( 4.780397808154266848, 1.280903732194421218, -8.968749997951611874 ) ) ;
#4254 = B_SPLINE_CURVE_WITH_KNOTS ( 'NONE', 3,
 ( #3003, #12321, #12514, #15221 ),
 .UNSPECIFIED., .F., .F.,
 ( 4, 4 ),
 ( 2.324263106244727961E-07, 0.0006888201370294844746 ),
 .UNSPECIFIED. ) ;
#4255 = VECTOR ( 'NONE', #15804, 1000.000000000000000 ) ;
#4256 = CARTESIAN_POINT ( 'NONE',  ( 2.031033467310412011, -24.32849926382740335, -12.98167595241049277 ) ) ;
#4257 = VERTEX_POINT ( 'NONE', #16349 ) ;
#4258 = CARTESIAN_POINT ( 'NONE',  ( 8.468749997951615427, -4.861323657744403448, -0.5109457054262123155 ) ) ;
#4259 = DIRECTION ( 'NONE',  ( 1.000000000000000000, 0.000000000000000000, 0.000000000000000000 ) ) ;
#4260 = CARTESIAN_POINT ( 'NONE',  ( -3.846120219227966430, -3.114526743279228072, -10.96874999795161720 ) ) ;
#4261 = EDGE_LOOP ( 'NONE', ( #10370, #6145, #6226, #4520 ) ) ;
#4262 = ORIENTED_EDGE ( 'NONE', *, *, #11018, .T. ) ;
#4263 = FACE_OUTER_BOUND ( 'NONE', #19069, .T. ) ;
#4264 = STYLED_ITEM ( 'NONE', ( #8422 ), #8048 ) ;
#4265 = CARTESIAN_POINT ( 'NONE',  ( 6.968749997951614539, 3.846120219227923798, 3.114526743279282694 ) ) ;
#4266 = ADVANCED_FACE ( 'NONE', ( #19441 ), #14566, .F. ) ;
#4267 = ORIENTED_EDGE ( 'NONE', *, *, #18874, .F. ) ;
#4268 = DIRECTION ( 'NONE',  ( -1.000000000000000000, -0.000000000000000000, -0.000000000000000000 ) ) ;
#4269 = ORIENTED_EDGE ( 'NONE', *, *, #18519, .F. ) ;
#4270 = LINE ( 'NONE', #14778, #14132 ) ;
#4271 = AXIS2_PLACEMENT_3D ( 'NONE', #15429, #9430, #18714 ) ;
#4272 = CARTESIAN_POINT ( 'NONE',  ( 0.07186814640506919427, -12.74240566898967764, -21.92302674874977697 ) ) ;
#4273 = EDGE_LOOP ( 'NONE', ( #2483, #6898, #4493, #3550 ) ) ;
#4274 = CARTESIAN_POINT ( 'NONE',  ( -3.255998204157480203, -17.85806462366060288, -32.00000000000000000 ) ) ;
#4275 = CYLINDRICAL_SURFACE ( 'NONE', #2956, 1.000000000000000888 ) ;
#4276 = CARTESIAN_POINT ( 'NONE',  ( 4.465502636338025688, -1.988169868018592856, -14.46874999795161720 ) ) ;
#4277 = ADVANCED_FACE ( 'NONE', ( #17658 ), #11842, .F. ) ;
#4278 = EDGE_CURVE ( 'NONE', #11503, #4614, #16254, .T. ) ;
#4279 = DIRECTION ( 'NONE',  ( -1.000000000000000000, -0.000000000000000000, -0.000000000000000000 ) ) ;
#4280 = CARTESIAN_POINT ( 'NONE',  ( -5.209999999999999964, 0.000000000000000000, 0.000000000000000000 ) ) ;
#4281 =( LENGTH_UNIT ( ) NAMED_UNIT ( * ) SI_UNIT ( .MILLI., .METRE. ) );
#4282 = DIRECTION ( 'NONE',  ( 0.000000000000000000, 0.000000000000000000, -1.000000000000000000 ) ) ;
#4283 = CIRCLE ( 'NONE', #2054, 6.000000000000000000 ) ;
#4284 = ORIENTED_EDGE ( 'NONE', *, *, #12312, .T. ) ;
#4285 = DIRECTION ( 'NONE',  ( 1.000000000000000000, 0.000000000000000000, 0.000000000000000000 ) ) ;
#4286 = FACE_BOUND ( 'NONE', #7271, .T. ) ;
#4287 = CARTESIAN_POINT ( 'NONE',  ( -3.143139765844555900, 4.840010801796527318, -12.50000000000000533 ) ) ;
#4288 = CARTESIAN_POINT ( 'NONE',  ( -2.602085213965210642E-14, -9.165435523385315975, -0.7089489049740167470 ) ) ;
#4289 = AXIS2_PLACEMENT_3D ( 'NONE', #13858, #17157, #5134 ) ;
#4290 = CARTESIAN_POINT ( 'NONE',  ( 13.00000000000000178, 4.545788521379996006, 1.798195097859992098 ) ) ;
#4291 = ORIENTED_EDGE ( 'NONE', *, *, #15396, .T. ) ;
#4292 = CARTESIAN_POINT ( 'NONE',  ( -9.671566133830877376, 15.77352024078954429, 35.00000000000000000 ) ) ;
#4293 = CARTESIAN_POINT ( 'NONE',  ( -2.000000000000001776, 0.000000000000000000, 7.500000000000000000 ) ) ;
#4294 = ORIENTED_EDGE ( 'NONE', *, *, #10908, .F. ) ;
#4295 = CARTESIAN_POINT ( 'NONE',  ( 10.31249999590322552, 0.5958122406255991210, 5.668774803599163192 ) ) ;
#4296 = VECTOR ( 'NONE', #2792, 1000.000000000000000 ) ;
#4297 = DIRECTION ( 'NONE',  ( 0.000000000000000000, 0.000000000000000000, 1.000000000000000000 ) ) ;
#4298 = CARTESIAN_POINT ( 'NONE',  ( 12.73273607671833929, 3.906077990787180099, -2.967013497616978412 ) ) ;
#4299 = CARTESIAN_POINT ( 'NONE',  ( 9.000000000000005329, 5.207209108562820710, 2.318398865532074193 ) ) ;
#4300 = ORIENTED_EDGE ( 'NONE', *, *, #11993, .F. ) ;
#4301 = MECHANICAL_DESIGN_GEOMETRIC_PRESENTATION_REPRESENTATION (  '', ( #150 ), #15492 ) ;
#4302 = FACE_OUTER_BOUND ( 'NONE', #6234, .T. ) ;
#4303 =( NAMED_UNIT ( * ) PLANE_ANGLE_UNIT ( ) SI_UNIT ( $, .RADIAN. ) );
#4304 = DIRECTION ( 'NONE',  ( -1.000000000000000000, 0.000000000000000000, 0.000000000000000000 ) ) ;
#4305 = LINE ( 'NONE', #10321, #7030 ) ;
#4306 = VERTEX_POINT ( 'NONE', #7317 ) ;
#4307 = CARTESIAN_POINT ( 'NONE',  ( -36.00000000000000000, 6.000000000000000888, 0.000000000000000000 ) ) ;
#4308 = ORIENTED_EDGE ( 'NONE', *, *, #5980, .T. ) ;
#4309 = DIRECTION ( 'NONE',  ( -0.000000000000000000, -0.000000000000000000, 1.000000000000000000 ) ) ;
#4310 = EDGE_CURVE ( 'NONE', #257, #226, #5974, .T. ) ;
#4311 = CARTESIAN_POINT ( 'NONE',  ( 9.468749997951615427, 3.954556930911862000, -2.873153789725825469 ) ) ;
#4312 = EDGE_CURVE ( 'NONE', #10459, #18268, #18765, .T. ) ;
#4313 = DIRECTION ( 'NONE',  ( 0.000000000000000000, 0.000000000000000000, 1.000000000000000000 ) ) ;
#4314 = LINE ( 'NONE', #12323, #16881 ) ;
#4315 = VERTEX_POINT ( 'NONE', #2437 ) ;
#4316 = CARTESIAN_POINT ( 'NONE',  ( -2.695436003842760275, -4.150607464521772094, -10.34374999795161543 ) ) ;
#4317 = DIRECTION ( 'NONE',  ( -1.000000000000000000, -1.224646799147353207E-16, 0.000000000000000000 ) ) ;
#4318 = CIRCLE ( 'NONE', #4644, 24.12539914357697768 ) ;
#4319 = ORIENTED_EDGE ( 'NONE', *, *, #12053, .F. ) ;
#4320 = ADVANCED_FACE ( 'NONE', ( #8553 ), #11648, .T. ) ;
#4321 = CARTESIAN_POINT ( 'NONE',  ( -14.19790265903626647, 9.644882309621941374, -35.00000000000000000 ) ) ;
#4322 = CARTESIAN_POINT ( 'NONE',  ( -2.246813503491864150, -4.409619785863891472, -13.34374999795161365 ) ) ;
#4323 = ADVANCED_FACE ( 'NONE', ( #1044 ), #11748, .T. ) ;
#4324 = VERTEX_POINT ( 'NONE', #13642 ) ;
#4325 =( REPRESENTATION_RELATIONSHIP ('NONE','NONE', #18211, #13463 ) REPRESENTATION_RELATIONSHIP_WITH_TRANSFORMATION ( #6235 )SHAPE_REPRESENTATION_RELATIONSHIP( ) );
#4326 = CARTESIAN_POINT ( 'NONE',  ( 0.5109457054261784537, 4.861323657744407001, -8.468749997951615427 ) ) ;
#4327 = CARTESIAN_POINT ( 'NONE',  ( 12.34374999795161543, 1.773574444220725743, 4.620319390059829168 ) ) ;
#4328 = EDGE_CURVE ( 'NONE', #11638, #16676, #10743, .T. ) ;
#4329 = CARTESIAN_POINT ( 'NONE',  ( 1.039999999999996705, -20.02152543075359503, 19.67366047555523423 ) ) ;
#4330 = ORIENTED_EDGE ( 'NONE', *, *, #4278, .F. ) ;
#4331 = CARTESIAN_POINT ( 'NONE',  ( 10.58013454126452046, -14.56230589874905412, 35.00000000000000000 ) ) ;
#4332 = ORIENTED_EDGE ( 'NONE', *, *, #5772, .F. ) ;
#4333 = DIRECTION ( 'NONE',  ( 0.000000000000000000, 0.000000000000000000, 1.000000000000000000 ) ) ;
#4334 = VECTOR ( 'NONE', #14147, 1000.000000000000000 ) ;
#4335 = ORIENTED_EDGE ( 'NONE', *, *, #12876, .F. ) ;
#4336 = SURFACE_SIDE_STYLE ('',( #16546 ) ) ;
#4337 = AXIS2_PLACEMENT_3D ( 'NONE', #15887, #5272, #4070 ) ;
#4338 = DIRECTION ( 'NONE',  ( 0.000000000000000000, 0.000000000000000000, -1.000000000000000000 ) ) ;
#4339 = CARTESIAN_POINT ( 'NONE',  ( 2.873153789725797491, -3.954556930911881985, -9.468749997951615427 ) ) ;
#4340 = CARTESIAN_POINT ( 'NONE',  ( 7.968749997951616315, -4.942249507334558700, 0.2590123213420631454 ) ) ;
#4341 = CARTESIAN_POINT ( 'NONE',  ( 9.468749997951615427, 4.465502636338023912, 1.988169868018593300 ) ) ;
#4342 = ORIENTED_EDGE ( 'NONE', *, *, #6423, .F. ) ;
#4343 = DIRECTION ( 'NONE',  ( -1.000000000000000000, -0.000000000000000000, -0.000000000000000000 ) ) ;
#4344 = LINE ( 'NONE', #10160, #19320 ) ;
#4345 = EDGE_CURVE ( 'NONE', #6099, #2546, #7417, .T. ) ;
#4346 = VECTOR ( 'NONE', #14837, 999.9999999999998863 ) ;
#4347 = VERTEX_POINT ( 'NONE', #9341 ) ;
#4348 = CIRCLE ( 'NONE', #15540, 7.500000000000000000 ) ;
#4349 = DIRECTION ( 'NONE',  ( -0.000000000000000000, -0.000000000000000000, 1.000000000000000000 ) ) ;
#4350 = CARTESIAN_POINT ( 'NONE',  ( 2.789999999999999147, 22.25075486061738772, 9.324097380959527115 ) ) ;
#4351 = EDGE_CURVE ( 'NONE', #15929, #8830, #12248, .T. ) ;
#4352 = CARTESIAN_POINT ( 'NONE',  ( -1.869200000000000195, 1.009010990753487416E-15, 8.239200000000002078 ) ) ;
#4353 = FACE_OUTER_BOUND ( 'NONE', #8058, .T. ) ;
#4354 = FACE_OUTER_BOUND ( 'NONE', #3257, .T. ) ;
#4355 = ORIENTED_EDGE ( 'NONE', *, *, #163, .F. ) ;
#4356 = CARTESIAN_POINT ( 'NONE',  ( -1.016293382781411125, 4.781284448697194378, -7.468749997951615427 ) ) ;
#4357 = ORIENTED_EDGE ( 'NONE', *, *, #7956, .F. ) ;
#4358 = DIRECTION ( 'NONE',  ( 1.000000000000000000, 0.000000000000000000, 0.000000000000000000 ) ) ;
#4359 = CARTESIAN_POINT ( 'NONE',  ( 2.849999999999954348, -4.936344801571327601, -6.000000000000005329 ) ) ;
#4360 = CARTESIAN_POINT ( 'NONE',  ( 1.749999999999998002, -4.633866840649122132, 27.68468304288257542 ) ) ;
#4361 = EDGE_LOOP ( 'NONE', ( #16146, #10357, #7440, #4495 ) ) ;
#4362 = VERTEX_POINT ( 'NONE', #16552 ) ;
#4363 = CARTESIAN_POINT ( 'NONE',  ( 5.510910596163084625E-16, 18.00000000000000355, -32.00000000000000000 ) ) ;
#4364 = VECTOR ( 'NONE', #15110, 1000.000000000000000 ) ;
#4365 = CARTESIAN_POINT ( 'NONE',  ( 13.50000000000000533, -5.574407415329169169, 1.493657965219485462 ) ) ;
#4366 = VERTEX_POINT ( 'NONE', #13541 ) ;
#4367 = CARTESIAN_POINT ( 'NONE',  ( 1.039999999999997593, 0.000000000000000000, 0.000000000000000000 ) ) ;
#4368 = ORIENTED_EDGE ( 'NONE', *, *, #1066, .T. ) ;
#4369 = DIRECTION ( 'NONE',  ( 1.000000000000000000, 0.000000000000000000, 0.000000000000000000 ) ) ;
#4370 = EDGE_CURVE ( 'NONE', #12759, #12346, #18780, .T. ) ;
#4371 = CARTESIAN_POINT ( 'NONE',  ( 1.039999999999995373, -12.96210679857767900, -24.89775460606846380 ) ) ;
#4372 = ORIENTED_EDGE ( 'NONE', *, *, #14387, .T. ) ;
#4373 = EDGE_CURVE ( 'NONE', #2730, #2350, #5794, .T. ) ;
#4374 = AXIS2_PLACEMENT_3D ( 'NONE', #15189, #7568, #9286 ) ;
#4375 = DIRECTION ( 'NONE',  ( 0.000000000000000000, -1.000000000000000000, 0.000000000000000000 ) ) ;
#4376 = CARTESIAN_POINT ( 'NONE',  ( 8.812499995903225525, 2.620002426024544029, -5.142044285764750811 ) ) ;
#4377 = CARTESIAN_POINT ( 'NONE',  ( -4.080749450109677490, -4.080749450109622423, -14.81249999590322375 ) ) ;
#4378 = ORIENTED_EDGE ( 'NONE', *, *, #12551, .F. ) ;
#4379 = CARTESIAN_POINT ( 'NONE',  ( 1.749999999999998002, 27.68468304288265358, -4.633866840648635410 ) ) ;
#4380 = SURFACE_STYLE_FILL_AREA ( #2973 ) ;
#4381 = VERTEX_POINT ( 'NONE', #13842 ) ;
#4382 = LINE ( 'NONE', #19685, #14640 ) ;
#4383 = FACE_BOUND ( 'NONE', #1657, .T. ) ;
#4384 = UNCERTAINTY_MEASURE_WITH_UNIT (LENGTH_MEASURE( 1.000000000000000082E-05 ), #6648, 'distance_accuracy_value', 'NONE');
#4385 = DIRECTION ( 'NONE',  ( 0.000000000000000000, 0.000000000000000000, 1.000000000000000000 ) ) ;
#4386 = CARTESIAN_POINT ( 'NONE',  ( -2.000000000000001776, 3.218695387886217230, -3.000000000000000000 ) ) ;
#4387 = CARTESIAN_POINT ( 'NONE',  ( -5.575441324182679459, 1.185096637661293251, -11.31249999590322375 ) ) ;
#4388 = EDGE_LOOP ( 'NONE', ( #54, #6373, #8795, #12731 ) ) ;
#4389 = DIRECTION ( 'NONE',  ( 1.000000000000000000, 0.000000000000000000, 0.000000000000000000 ) ) ;
#4390 = EDGE_CURVE ( 'NONE', #4589, #18335, #18461, .T. ) ;
#4391 = CARTESIAN_POINT ( 'NONE',  ( -3.114526743279308896, -3.846120219227900705, -6.968749997951614539 ) ) ;
#4392 = ORIENTED_EDGE ( 'NONE', *, *, #10326, .T. ) ;
#4393 = DIRECTION ( 'NONE',  ( 0.000000000000000000, 0.000000000000000000, 1.000000000000000000 ) ) ;
#4394 = DIRECTION ( 'NONE',  ( 0.000000000000000000, 0.000000000000000000, 1.000000000000000000 ) ) ;
#4395 = EDGE_CURVE ( 'NONE', #4149, #6896, #5109, .T. ) ;
#4396 = CARTESIAN_POINT ( 'NONE',  ( 6.968749997951614539, -3.846120219227900705, -3.114526743279308896 ) ) ;
#4397 = CARTESIAN_POINT ( 'NONE',  ( 8.500000000000005329, 5.574407415329157622, 1.493657965219523875 ) ) ;
#4398 = ORIENTED_EDGE ( 'NONE', *, *, #18708, .F. ) ;
#4399 = CIRCLE ( 'NONE', #19093, 8.000000000000000000 ) ;
#4400 = CARTESIAN_POINT ( 'NONE',  ( -36.00000000000000000, -2.000000000000000888, -5.000000000000000000 ) ) ;
#4401 = SURFACE_SIDE_STYLE ('',( #12009 ) ) ;
#4402 = DIRECTION ( 'NONE',  ( 0.000000000000000000, -1.000000000000000000, 0.000000000000000000 ) ) ;
#4403 = CARTESIAN_POINT ( 'NONE',  ( 14.00000000000000533, -3.350375938067065906, -4.611396867937224364 ) ) ;
#4404 = EDGE_LOOP ( 'NONE', ( #8244, #6068, #17246, #145 ) ) ;
#4405 = DIRECTION ( 'NONE',  ( -1.000000000000000000, 0.000000000000000000, -0.000000000000000000 ) ) ;
#4406 = ORIENTED_EDGE ( 'NONE', *, *, #12150, .F. ) ;
#4407 = DIRECTION ( 'NONE',  ( -1.000000000000000000, 0.000000000000000000, 0.000000000000000000 ) ) ;
#4408 = FACE_OUTER_BOUND ( 'NONE', #1316, .T. ) ;
#4409 = CARTESIAN_POINT ( 'NONE',  ( 2.604434261026087771, 25.39738473785002526, 5.253342437939815923 ) ) ;
#4410 = DIRECTION ( 'NONE',  ( 0.000000000000000000, 6.982962677686267499E-15, -1.000000000000000000 ) ) ;
#4411 = ORIENTED_EDGE ( 'NONE', *, *, #2579, .F. ) ;
#4412 = DIRECTION ( 'NONE',  ( 0.000000000000000000, 0.000000000000000000, 1.000000000000000000 ) ) ;
#4413 = EDGE_CURVE ( 'NONE', #10153, #12571, #7827, .T. ) ;
#4414 = CARTESIAN_POINT ( 'NONE',  ( -5.209999999999999964, 0.000000000000000000, 0.000000000000000000 ) ) ;
#4415 = AXIS2_PLACEMENT_3D ( 'NONE', #13094, #17695, #18093 ) ;
#4416 = ORIENTED_EDGE ( 'NONE', *, *, #13372, .F. ) ;
#4417 = AXIS2_PLACEMENT_3D ( 'NONE', #6955, #681, #16188 ) ;
#4418 = EDGE_CURVE ( 'NONE', #6896, #10630, #19163, .T. ) ;
#4419 = DIRECTION ( 'NONE',  ( 0.000000000000000000, 0.000000000000000000, 1.000000000000000000 ) ) ;
#4420 = EDGE_CURVE ( 'NONE', #11638, #19481, #14883, .T. ) ;
#4421 = ORIENTED_EDGE ( 'NONE', *, *, #8366, .T. ) ;
#4422 = CARTESIAN_POINT ( 'NONE',  ( 4.781284448697194378, 1.016293382781411792, -12.84374999795161543 ) ) ;
#4423 = DIRECTION ( 'NONE',  ( 0.000000000000000000, 0.000000000000000000, -1.000000000000000000 ) ) ;
#4424 = DIRECTION ( 'NONE',  ( 4.060088635510494296E-15, -1.000000000000000000, 0.000000000000000000 ) ) ;
#4425 = ORIENTED_EDGE ( 'NONE', *, *, #6029, .F. ) ;
#4426 = DIRECTION ( 'NONE',  ( -1.000000000000000000, 0.000000000000000000, 0.000000000000000000 ) ) ;
#4427 = ORIENTED_EDGE ( 'NONE', *, *, #10847, .T. ) ;
#4429 = CYLINDRICAL_SURFACE ( 'NONE', #7246, 4.000000000000000000 ) ;
#4428 = AXIS2_PLACEMENT_3D ( 'NONE', #19664, #17976, #2549 ) ;
#4430 = VERTEX_POINT ( 'NONE', #12147 ) ;
#4431 = CYLINDRICAL_SURFACE ( 'NONE', #3834, 3.968750000000000000 ) ;
#4432 = CARTESIAN_POINT ( 'NONE',  ( 2.724444381390116021, -21.84113606038314259, 12.72236714503155142 ) ) ;
#4433 = ADVANCED_FACE ( 'NONE', ( #4531 ), #6317, .T. ) ;
#4434 = EDGE_CURVE ( 'NONE', #18092, #1561, #3526, .T. ) ;
#4435 = CARTESIAN_POINT ( 'NONE',  ( 8.671566133830875600, 15.77352024078954784, 35.00000000000000000 ) ) ;
#4436 = CARTESIAN_POINT ( 'NONE',  ( 8.671566133830875600, 15.77352024078954784, 32.00000000000000000 ) ) ;
#4437 = CARTESIAN_POINT ( 'NONE',  ( 13.00000000000000533, 4.560365019702147471, 2.978280878416429633 ) ) ;
#4438 = AXIS2_PLACEMENT_3D ( 'NONE', #3047, #4358, #2946 ) ;
#4439 = VERTEX_POINT ( 'NONE', #14236 ) ;
#4440 = CARTESIAN_POINT ( 'NONE',  ( 0.000000000000000000, 20.62201879784932856, -12.52067188844328705 ) ) ;
#4441 = EDGE_CURVE ( 'NONE', #4236, #941, #6747, .T. ) ;
#4442 = DIRECTION ( 'NONE',  ( 0.000000000000000000, 0.000000000000000000, 1.000000000000000000 ) ) ;
#4443 = TOROIDAL_SURFACE ( 'NONE', #17854, 24.12539914357697413, 8.000000000000000000 ) ;
#4444 = EDGE_LOOP ( 'NONE', ( #11937, #7019 ) ) ;
#4445 = CARTESIAN_POINT ( 'NONE',  ( -14.00000000000000178, 0.000000000000000000, 35.00000000000000000 ) ) ;
#4446 = CARTESIAN_POINT ( 'NONE',  ( 1.899999999999999023, 0.000000000000000000, 0.000000000000000000 ) ) ;
#4447 = VERTEX_POINT ( 'NONE', #8229 ) ;
#4448 = DIRECTION ( 'NONE',  ( 0.000000000000000000, 0.000000000000000000, -1.000000000000000000 ) ) ;
#4449 = CARTESIAN_POINT ( 'NONE',  ( 1.280903732194421663, -4.780397808154265960, -13.96874999795161365 ) ) ;
#4450 = CARTESIAN_POINT ( 'NONE',  ( -14.86923836996421144, -11.47363181547641275, -32.00000000000000000 ) ) ;
#4451 = PLANE ( 'NONE',  #9050 ) ;
#4452 = ORIENTED_EDGE ( 'NONE', *, *, #1066, .F. ) ;
#4453 = CARTESIAN_POINT ( 'NONE',  ( 9.468749997951615427, -4.465502636338009701, -1.988169868018624609 ) ) ;
#4454 = ORIENTED_EDGE ( 'NONE', *, *, #17752, .F. ) ;
#4455 = CARTESIAN_POINT ( 'NONE',  ( 0.000000000000000000, 0.000000000000000000, 0.000000000000000000 ) ) ;
#4456 = CARTESIAN_POINT ( 'NONE',  ( 5.575441324182695446, 1.185096637661215757, -12.00000000000000533 ) ) ;
#4457 = CARTESIAN_POINT ( 'NONE',  ( 1.039999999999997593, 0.000000000000000000, 0.000000000000000000 ) ) ;
#4458 = EDGE_CURVE ( 'NONE', #253, #1013, #2793, .T. ) ;
#4459 = VERTEX_POINT ( 'NONE', #18730 ) ;
#4460 = ORIENTED_EDGE ( 'NONE', *, *, #3164, .T. ) ;
#4461 = DIRECTION ( 'NONE',  ( -0.000000000000000000, -0.000000000000000000, 1.000000000000000000 ) ) ;
#4462 = CARTESIAN_POINT ( 'NONE',  ( 1.749999999999998002, -4.147968289691086774, -27.76164181293056288 ) ) ;
#4463 = ORIENTED_EDGE ( 'NONE', *, *, #1887, .T. ) ;
#4464 = PRESENTATION_LAYER_ASSIGNMENT (  '', '', ( #13089 ) ) ;
#4465 = FACE_OUTER_BOUND ( 'NONE', #7126, .T. ) ;
#4466 = VERTEX_POINT ( 'NONE', #12439 ) ;
#4467 = CARTESIAN_POINT ( 'NONE',  ( 6.000593838912648081, -0.002144393866035136480, 5.699999596629369059 ) ) ;
#4468 = VERTEX_POINT ( 'NONE', #3727 ) ;
#4469 = CARTESIAN_POINT ( 'NONE',  ( 2.444050593749960587, -4.233219804643904460, -6.843749997951615427 ) ) ;
#4470 = DIRECTION ( 'NONE',  ( 0.000000000000000000, 0.000000000000000000, -1.000000000000000000 ) ) ;
#4471 = LINE ( 'NONE', #10583, #15160 ) ;
#4472 = ORIENTED_EDGE ( 'NONE', *, *, #16768, .F. ) ;
#4473 = CARTESIAN_POINT ( 'NONE',  ( 6.234374998975811266, -3.696815770993907903E-14, 5.294050593750000644 ) ) ;
#4474 = CIRCLE ( 'NONE', #1280, 12.00000000000000178 ) ;
#4475 = DIRECTION ( 'NONE',  ( 0.000000000000000000, 0.000000000000000000, -1.000000000000000000 ) ) ;
#4476 = EDGE_LOOP ( 'NONE', ( #4651, #2073, #218, #5103 ) ) ;
#4477 = CYLINDRICAL_SURFACE ( 'NONE', #6626, 0.9999999999999974465 ) ;
#4478 = DIRECTION ( 'NONE',  ( -1.000000000000000000, 0.000000000000000000, 0.000000000000000000 ) ) ;
#4479 = DIRECTION ( 'NONE',  ( 1.000000000000000000, 0.000000000000000000, 0.000000000000000000 ) ) ;
#4480 = DIRECTION ( 'NONE',  ( -1.000000000000000000, 0.000000000000000000, 0.000000000000000000 ) ) ;
#4481 = CARTESIAN_POINT ( 'NONE',  ( 0.006974663525958337516, -12.53640742967767885, 21.08118142846899801 ) ) ;
#4482 = ADVANCED_FACE ( 'NONE', ( #3431 ), #5223, .T. ) ;
#4483 = ORIENTED_EDGE ( 'NONE', *, *, #15845, .T. ) ;
#4484 = LINE ( 'NONE', #7674, #14457 ) ;
#4485 = DIRECTION ( 'NONE',  ( 1.000000000000000000, 0.000000000000000000, 0.000000000000000000 ) ) ;
#4486 = VECTOR ( 'NONE', #4479, 1000.000000000000000 ) ;
#4487 = EDGE_LOOP ( 'NONE', ( #16822, #9810, #13995, #9536 ) ) ;
#4488 = CARTESIAN_POINT ( 'NONE',  ( 12.31249999590322552, -2.850000000000023626, 4.936344801571289409 ) ) ;
#4489 = CARTESIAN_POINT ( 'NONE',  ( -14.00000000000000178, 0.000000000000000000, 32.00000000000000000 ) ) ;
#4490 = ADVANCED_FACE ( 'NONE', ( #9642 ), #2950, .T. ) ;
#4491 = CARTESIAN_POINT ( 'NONE',  ( 10.46874999795161720, 1.016293382781477961, -4.781284448697179279 ) ) ;
#4492 = CARTESIAN_POINT ( 'NONE',  ( -1.303212546021025764, -8.413025409128790599, -0.3142460757452265052 ) ) ;
#4493 = ORIENTED_EDGE ( 'NONE', *, *, #11877, .T. ) ;
#4494 = CARTESIAN_POINT ( 'NONE',  ( 0.000000000000000000, 18.28042085475278000, 15.74360496233386719 ) ) ;
#4495 = ORIENTED_EDGE ( 'NONE', *, *, #3198, .F. ) ;
#4496 = CARTESIAN_POINT ( 'NONE',  ( -17.68117051311639898, -3.372863662543042818, 32.00000000000000000 ) ) ;
#4497 = AXIS2_PLACEMENT_3D ( 'NONE', #10023, #19014, #18910 ) ;
#4498 = CARTESIAN_POINT ( 'NONE',  ( 2.789999999999999147, -7.909232158574647009, -24.34211360614308006 ) ) ;
#4499 = DIRECTION ( 'NONE',  ( 0.000000000000000000, -3.552713678800500929E-15, 1.000000000000000000 ) ) ;
#4500 = CARTESIAN_POINT ( 'NONE',  ( 7.843749997951614539, 1.510506337161861445, -4.648860486681953397 ) ) ;
#4501 = DIRECTION ( 'NONE',  ( 0.000000000000000000, 0.000000000000000000, 1.000000000000000000 ) ) ;
#4502 = DIRECTION ( 'NONE',  ( -0.000000000000000000, -0.000000000000000000, 1.000000000000000000 ) ) ;
#4503 = EDGE_CURVE ( 'NONE', #13431, #12853, #1670, .T. ) ;
#4504 = EDGE_LOOP ( 'NONE', ( #12554, #11362, #5384, #7813, #5435 ) ) ;
#4505 = CARTESIAN_POINT ( 'NONE',  ( 2.789999999999999147, 0.2301004812061083760, -24.44424927289185234 ) ) ;
#4506 = CARTESIAN_POINT ( 'NONE',  ( 0.1855656748306453718, 25.77772010606605946, 2.851997810081739360 ) ) ;
#4507 = VERTEX_POINT ( 'NONE', #5417 ) ;
#4508 = VECTOR ( 'NONE', #9052, 1000.000000000000000 ) ;
#4509 = CIRCLE ( 'NONE', #1001, 28.06981291497571362 ) ;
#4510 = CIRCLE ( 'NONE', #16022, 6.000000000000000000 ) ;
#4511 = CARTESIAN_POINT ( 'NONE',  ( -4.888101187500000222, 0.000000000000000000, -6.468749997951615427 ) ) ;
#4512 = CARTESIAN_POINT ( 'NONE',  ( 4.409619785863891472, -2.246813503491864150, -8.343749997951613651 ) ) ;
#4513 = ORIENTED_EDGE ( 'NONE', *, *, #5448, .T. ) ;
#4514 = CARTESIAN_POINT ( 'NONE',  ( 2.695436003842732298, 4.150607464521791634, -9.968749997951617203 ) ) ;
#4515 = CARTESIAN_POINT ( 'NONE',  ( 13.81249999590322552, 0.3020334839682480288, 5.763142191869157216 ) ) ;
#4516 = CARTESIAN_POINT ( 'NONE',  ( 1.039999999999997371, 25.12109765559653596, 12.52377138324232675 ) ) ;
#4517 = EDGE_LOOP ( 'NONE', ( #13105, #6804 ) ) ;
#4518 = EDGE_CURVE ( 'NONE', #11655, #4548, #16235, .T. ) ;
#4519 = FACE_OUTER_BOUND ( 'NONE', #5574, .T. ) ;
#4520 = ORIENTED_EDGE ( 'NONE', *, *, #19468, .F. ) ;
#4521 = EDGE_CURVE ( 'NONE', #3152, #18644, #6300, .T. ) ;
#4522 = CARTESIAN_POINT ( 'NONE',  ( -4.643890550183624732, -6.484284064149645310, -0.01675691374233593753 ) ) ;
#4523 = ORIENTED_EDGE ( 'NONE', *, *, #13649, .T. ) ;
#4524 = DIRECTION ( 'NONE',  ( 0.000000000000000000, 0.000000000000000000, 1.000000000000000000 ) ) ;
#4525 = DIRECTION ( 'NONE',  ( 0.000000000000000000, -1.000000000000000000, 0.000000000000000000 ) ) ;
#4526 = DIRECTION ( 'NONE',  ( 0.000000000000000000, 0.000000000000000000, -1.000000000000000000 ) ) ;
#4527 = DIRECTION ( 'NONE',  ( 0.000000000000000000, 0.000000000000000000, -1.000000000000000000 ) ) ;
#4528 = EDGE_CURVE ( 'NONE', #809, #2904, #13228, .T. ) ;
#4529 = AXIS2_PLACEMENT_3D ( 'NONE', #10139, #19423, #16237 ) ;
#4530 = AXIS2_PLACEMENT_3D ( 'NONE', #4505, #15228, #4412 ) ;
#4531 = FACE_OUTER_BOUND ( 'NONE', #3620, .T. ) ;
#4532 = EDGE_LOOP ( 'NONE', ( #1737, #3250, #8557, #3766 ) ) ;
#4533 = CIRCLE ( 'NONE', #10609, 1.000000000000004441 ) ;
#4534 = CARTESIAN_POINT ( 'NONE',  ( 2.000000000000001776, 0.000000000000000000, -8.073750000000021743 ) ) ;
#4535 = EDGE_CURVE ( 'NONE', #12710, #9399, #1539, .T. ) ;
#4536 = FILL_AREA_STYLE_COLOUR ( '', #7810 ) ;
#4537 = AXIS2_PLACEMENT_3D ( 'NONE', #19774, #13478, #6067 ) ;
#4538 = VERTEX_POINT ( 'NONE', #3822 ) ;
#4539 = FACE_OUTER_BOUND ( 'NONE', #17616, .T. ) ;
#4540 = LINE ( 'NONE', #15053, #7761 ) ;
#4541 = ORIENTED_EDGE ( 'NONE', *, *, #6214, .T. ) ;
#4542 = CIRCLE ( 'NONE', #17648, 9.000000000000021316 ) ;
#4543 = DIRECTION ( 'NONE',  ( 0.000000000000000000, 0.000000000000000000, 1.000000000000000000 ) ) ;
#4544 = CIRCLE ( 'NONE', #13482, 2.524999999999995914 ) ;
#4545 = CARTESIAN_POINT ( 'NONE',  ( 5.387740456496221242, -2.068159791354221344, -10.50000000000000711 ) ) ;
#4546 = AXIS2_PLACEMENT_3D ( 'NONE', #7777, #183, #277 ) ;
#4547 = CYLINDRICAL_SURFACE ( 'NONE', #10342, 1.000000000000003109 ) ;
#4548 = VERTEX_POINT ( 'NONE', #10230 ) ;
#4549 = CARTESIAN_POINT ( 'NONE',  ( 2.789999999999999147, 1.991882183130294637, 24.04302995059966364 ) ) ;
#4550 = DIRECTION ( 'NONE',  ( -8.326672684688674053E-17, 8.326672684688674053E-17, -1.000000000000000000 ) ) ;
#4551 = CARTESIAN_POINT ( 'NONE',  ( 2.765633920072235963, -5.391175441198450713, -24.15498966839968276 ) ) ;
#4552 = CARTESIAN_POINT ( 'NONE',  ( -5.387740456496247887, -2.068159791354146293, -12.81249999590322552 ) ) ;
#4553 = VECTOR ( 'NONE', #18423, 1000.000000000000000 ) ;
#4554 = CIRCLE ( 'NONE', #18298, 28.06981291497571362 ) ;
#4555 = ORIENTED_EDGE ( 'NONE', *, *, #17741, .F. ) ;
#4556 = ORIENTED_EDGE ( 'NONE', *, *, #13741, .F. ) ;
#4557 = CARTESIAN_POINT ( 'NONE',  ( 2.789999999999999147, 15.74360496233381390, 18.28042085475283685 ) ) ;
#4558 = CARTESIAN_POINT ( 'NONE',  ( 11.84374999795161365, 4.888101187500000222, -2.993098736590125853E-16 ) ) ;
#4559 = ORIENTED_EDGE ( 'NONE', *, *, #4243, .F. ) ;
#4560 = EDGE_CURVE ( 'NONE', #12621, #18193, #1851, .T. ) ;
#4561 = EDGE_CURVE ( 'NONE', #2407, #6506, #2479, .T. ) ;
#4562 = CARTESIAN_POINT ( 'NONE',  ( 15.19790265903627358, 9.644882309621939598, 32.00000000000000000 ) ) ;
#4563 = VERTEX_POINT ( 'NONE', #8619 ) ;
#4564 = LINE ( 'NONE', #3159, #10938 ) ;
#4565 = AXIS2_PLACEMENT_3D ( 'NONE', #9545, #1634, #18538 ) ;
#4566 = ORIENTED_EDGE ( 'NONE', *, *, #4458, .F. ) ;
#4567 = AXIS2_PLACEMENT_3D ( 'NONE', #1642, #7735, #8951 ) ;
#4568 = EDGE_CURVE ( 'NONE', #720, #18915, #16032, .T. ) ;
#4569 = AXIS2_PLACEMENT_3D ( 'NONE', #4498, #13909, #8640 ) ;
#4570 = CARTESIAN_POINT ( 'NONE',  ( 2.765633920072235519, 9.836394144776026138, -22.71065055754441531 ) ) ;
#4571 = CARTESIAN_POINT ( 'NONE',  ( 10.31249999590322552, 4.611396867937201272, -3.350375938067097437 ) ) ;
#4572 = CARTESIAN_POINT ( 'NONE',  ( 0.000000000000000000, 0.000000000000000000, 35.00000000000000000 ) ) ;
#4573 = ADVANCED_FACE ( 'NONE', ( #10041 ), #2605, .F. ) ;
#4574 = VECTOR ( 'NONE', #525, 1000.000000000000000 ) ;
#4575 = ORIENTED_EDGE ( 'NONE', *, *, #15258, .T. ) ;
#4576 = LINE ( 'NONE', #12180, #11421 ) ;
#4577 = ADVANCED_FACE ( 'NONE', ( #5512, #19218 ), #7003, .T. ) ;
#4578 = DIRECTION ( 'NONE',  ( 0.000000000000000000, 0.000000000000000000, 1.000000000000000000 ) ) ;
#4579 = VERTEX_POINT ( 'NONE', #11622 ) ;
#4580 = CARTESIAN_POINT ( 'NONE',  ( 2.262072625383134472, 4.996265754456739927, -26.57710921259756631 ) ) ;
#4581 = FACE_BOUND ( 'NONE', #7700, .T. ) ;
#4582 = CARTESIAN_POINT ( 'NONE',  ( 111.3234999999999957, 0.000000000000000000, 4.000000000000000000 ) ) ;
#4583 = AXIS2_PLACEMENT_3D ( 'NONE', #19300, #17810, #11609 ) ;
#4584 = CARTESIAN_POINT ( 'NONE',  ( 12.86923836996420967, -11.47363181547641453, 32.00000000000000000 ) ) ;
#4585 = CARTESIAN_POINT ( 'NONE',  ( -7.770166132776744975E-14, -12.51293083811813389, 20.85287692521926672 ) ) ;
#4586 = VERTEX_POINT ( 'NONE', #11817 ) ;
#4587 = DIRECTION ( 'NONE',  ( 1.000000000000000000, 0.000000000000000000, 0.000000000000000000 ) ) ;
#4588 = FACE_OUTER_BOUND ( 'NONE', #6816, .T. ) ;
#4589 = VERTEX_POINT ( 'NONE', #13033 ) ;
#4590 = CARTESIAN_POINT ( 'NONE',  ( 10.50000000000000711, 2.068159791354259092, -5.387740456496206143 ) ) ;
#4591 = EDGE_CURVE ( 'NONE', #13534, #18366, #7264, .T. ) ;
#4592 = CARTESIAN_POINT ( 'NONE',  ( -5.700000000000001066, 0.2987243419133610023, -14.14705514798868435 ) ) ;
#4593 = B_SPLINE_CURVE_WITH_KNOTS ( 'NONE', 3,
 ( #3185, #3286, #9298, #15400, #1694, #18493 ),
 .UNSPECIFIED., .F., .F.,
 ( 4, 2, 4 ),
 ( 0.01281224986012821990, 0.01513166665602956075, 0.01745108345193090160 ),
 .UNSPECIFIED. ) ;
#4594 = B_SPLINE_CURVE_WITH_KNOTS ( 'NONE', 3,
 ( #10964, #12168, #12266, #18368, #3154, #3357 ),
 .UNSPECIFIED., .F., .F.,
 ( 4, 2, 4 ),
 ( 4.462636882221166670E-07, 0.001879885203074802827, 0.003759324142461383488 ),
 .UNSPECIFIED. ) ;
#4595 = AXIS2_PLACEMENT_3D ( 'NONE', #18890, #6865, #8390 ) ;
#4596 = DIRECTION ( 'NONE',  ( 0.000000000000000000, 0.000000000000000000, -1.000000000000000000 ) ) ;
#4597 = DIRECTION ( 'NONE',  ( -1.000000000000000000, 0.000000000000000000, 0.000000000000000000 ) ) ;
#4598 = EDGE_LOOP ( 'NONE', ( #11633, #7719, #10405, #12702 ) ) ;
#4599 = EDGE_CURVE ( 'NONE', #9729, #19421, #1220, .T. ) ;
#4600 = CARTESIAN_POINT ( 'NONE',  ( 2.999999999999998224, 2.487173708821167839, -2.318181818181817899 ) ) ;
#4601 = SURFACE_SIDE_STYLE ('',( #5894 ) ) ;
#4602 = DIRECTION ( 'NONE',  ( -1.000000000000000000, 0.000000000000000000, 0.000000000000000000 ) ) ;
#4603 = EDGE_CURVE ( 'NONE', #750, #1730, #18150, .T. ) ;
#4604 = CYLINDRICAL_SURFACE ( 'NONE', #14396, 28.06981291497571362 ) ;
#4605 = VERTEX_POINT ( 'NONE', #19511 ) ;
#4606 = LINE ( 'NONE', #16518, #247 ) ;
#4607 = AXIS2_PLACEMENT_3D ( 'NONE', #5571, #11681, #13375 ) ;
#4608 = CARTESIAN_POINT ( 'NONE',  ( 2.789999999999999147, 7.909232158575156824, -24.34211360614291664 ) ) ;
#4609 = CARTESIAN_POINT ( 'NONE',  ( 1.039999999999996261, 24.89775460606850999, -12.96210679857759018 ) ) ;
#4610 = DIRECTION ( 'NONE',  ( 1.000000000000000000, 0.000000000000000000, 0.000000000000000000 ) ) ;
#4611 = ORIENTED_EDGE ( 'NONE', *, *, #13125, .T. ) ;
#4612 = CARTESIAN_POINT ( 'NONE',  ( 0.000000000000000000, 0.000000000000000000, 0.000000000000000000 ) ) ;
#4613 = EDGE_CURVE ( 'NONE', #7394, #2993, #15324, .T. ) ;
#4614 = VERTEX_POINT ( 'NONE', #1516 ) ;
#4615 = CARTESIAN_POINT ( 'NONE',  ( 7.343749997951615427, -0.7741991708319229115, 4.888101187499994893 ) ) ;
#4616 = CYLINDRICAL_SURFACE ( 'NONE', #15853, 2.524999999999995914 ) ;
#4617 = VERTEX_POINT ( 'NONE', #4710 ) ;
#4618 = CARTESIAN_POINT ( 'NONE',  ( -2.873153789725825469, 3.954556930911862000, -9.843749997951615427 ) ) ;
#4619 = DIRECTION ( 'NONE',  ( 1.000000000000000000, 0.000000000000000000, 0.000000000000000000 ) ) ;
#4620 = ORIENTED_EDGE ( 'NONE', *, *, #13728, .T. ) ;
#4621 = CARTESIAN_POINT ( 'NONE',  ( 0.000000000000000000, 0.000000000000000000, 0.000000000000000000 ) ) ;
#4622 = CARTESIAN_POINT ( 'NONE',  ( 14.86923836996420434, -11.47363181547641453, -35.00000000000000000 ) ) ;
#4623 = EDGE_CURVE ( 'NONE', #14183, #4945, #4314, .T. ) ;
#4624 = AXIS2_PLACEMENT_3D ( 'NONE', #6087, #3094, #12010 ) ;
#4625 = VERTEX_POINT ( 'NONE', #7699 ) ;
#4626 = CARTESIAN_POINT ( 'NONE',  ( -4.476417968967385974, 17.43449690031536292, -32.00000000000000000 ) ) ;
#4627 = EDGE_LOOP ( 'NONE', ( #1062, #10444, #14744, #254 ) ) ;
#4628 = CARTESIAN_POINT ( 'NONE',  ( -4.305564957446068597, -6.679616436190415563, -1.463672932855429408E-15 ) ) ;
#4629 = VERTEX_POINT ( 'NONE', #10718 ) ;
#4630 = CARTESIAN_POINT ( 'NONE',  ( 2.789999999999999147, 20.62201879784931435, -12.52067188844328882 ) ) ;
#4631 = DIRECTION ( 'NONE',  ( 0.000000000000000000, 0.000000000000000000, 1.000000000000000000 ) ) ;
#4632 = CARTESIAN_POINT ( 'NONE',  ( 6.929096493834647319, 2.870125742738179664, 12.00000000000000000 ) ) ;
#4633 = DIRECTION ( 'NONE',  ( -1.000000000000000000, -6.419766481290786633E-33, 0.000000000000000000 ) ) ;
#4634 = CARTESIAN_POINT ( 'NONE',  ( 6.968749997951614539, 4.620319390059829168, -1.773574444220725077 ) ) ;
#4635 = ORIENTED_EDGE ( 'NONE', *, *, #2705, .F. ) ;
#4636 = CARTESIAN_POINT ( 'NONE',  ( 0.02436607992776455150, 21.30679549418631780, 12.59161484032919986 ) ) ;
#4637 = EDGE_CURVE ( 'NONE', #19430, #18625, #19422, .T. ) ;
#4638 = DIRECTION ( 'NONE',  ( -1.000000000000000000, 0.000000000000000000, 0.000000000000000000 ) ) ;
#4639 = ADVANCED_FACE ( 'NONE', ( #15120 ), #1213, .F. ) ;
#4640 = ORIENTED_EDGE ( 'NONE', *, *, #12744, .F. ) ;
#4641 = CYLINDRICAL_SURFACE ( 'NONE', #13787, 5.400000000000000355 ) ;
#4642 = DIRECTION ( 'NONE',  ( -1.000000000000000000, -0.000000000000000000, -0.000000000000000000 ) ) ;
#4643 = ORIENTED_EDGE ( 'NONE', *, *, #12019, .F. ) ;
#4644 = AXIS2_PLACEMENT_3D ( 'NONE', #3979, #17586, #18785 ) ;
#4645 = DIRECTION ( 'NONE',  ( 0.000000000000000000, 0.000000000000000000, 1.000000000000000000 ) ) ;
#4646 = CARTESIAN_POINT ( 'NONE',  ( 0.5958122406255995651, -5.668774803599162304, -14.00000000000000533 ) ) ;
#4647 = EDGE_CURVE ( 'NONE', #1354, #8320, #8442, .T. ) ;
#4649 = EDGE_CURVE ( 'NONE', #14057, #11278, #2190, .T. ) ;
#4648 = CIRCLE ( 'NONE', #7177, 28.06981291497571362 ) ;
#4650 =( LENGTH_UNIT ( ) NAMED_UNIT ( * ) SI_UNIT ( .MILLI., .METRE. ) );
#4651 = ORIENTED_EDGE ( 'NONE', *, *, #12165, .F. ) ;
#4652 = SHAPE_REPRESENTATION ( 'plain washer clevis pin grade a_iso_ISO 8738 - 8', ( #16724 ), #279 ) ;
#4653 = CARTESIAN_POINT ( 'NONE',  ( 3.846120219227944670, 3.114526743279255161, -10.96874999795161720 ) ) ;
#4654 = ORIENTED_EDGE ( 'NONE', *, *, #14920, .F. ) ;
#4655 = PRODUCT_CONTEXT ( 'NONE', #15199, 'mechanical' ) ;
#4656 = DIRECTION ( 'NONE',  ( -1.000000000000000000, 0.000000000000000000, 0.000000000000000000 ) ) ;
#4657 = DIRECTION ( 'NONE',  ( 0.000000000000000000, 0.000000000000000000, 1.000000000000000000 ) ) ;
#4658 = VERTEX_POINT ( 'NONE', #8818 ) ;
#4659 = VERTEX_POINT ( 'NONE', #14923 ) ;
#4660 = CARTESIAN_POINT ( 'NONE',  ( -0.2590123213420975623, 4.942249507334556924, -8.343749997951611874 ) ) ;
#4661 = VERTEX_POINT ( 'NONE', #13412 ) ;
#4662 = CIRCLE ( 'NONE', #8494, 6.200000000000020606 ) ;
#4663 = CIRCLE ( 'NONE', #16494, 0.9999999999999974465 ) ;
#4664 = PRESENTATION_STYLE_ASSIGNMENT (( #18371 ) ) ;
#4665 = PRODUCT_RELATED_PRODUCT_CATEGORY ( 'part', '', ( #17690 ) ) ;
#4666 = ORIENTED_EDGE ( 'NONE', *, *, #19645, .F. ) ;
#4667 = EDGE_CURVE ( 'NONE', #18721, #3997, #5800, .T. ) ;
#4668 = DIRECTION ( 'NONE',  ( 0.000000000000000000, -1.000000000000000000, 0.000000000000000000 ) ) ;
#4669 = DIRECTION ( 'NONE',  ( 0.000000000000000000, 0.000000000000000000, 1.000000000000000000 ) ) ;
#4670 = CARTESIAN_POINT ( 'NONE',  ( -4.611396867937224364, -3.350375938067065906, -15.31249999590322552 ) ) ;
#4671 = ADVANCED_FACE ( 'NONE', ( #4 ), #8917, .T. ) ;
#4672 = AXIS2_PLACEMENT_3D ( 'NONE', #10344, #4423, #15132 ) ;
#4673 = ORIENTED_EDGE ( 'NONE', *, *, #9703, .T. ) ;
#4674 = ORIENTED_EDGE ( 'NONE', *, *, #12667, .F. ) ;
#4675 = DIRECTION ( 'NONE',  ( 0.000000000000000000, 0.000000000000000000, 1.000000000000000000 ) ) ;
#4676 = LINE ( 'NONE', #16889, #5832 ) ;
#4677 = CIRCLE ( 'NONE', #6245, 0.1999999999999987899 ) ;
#4678 = ORIENTED_EDGE ( 'NONE', *, *, #10655, .F. ) ;
#4679 = DIRECTION ( 'NONE',  ( 1.000000000000000000, 6.419766481290786633E-33, -0.000000000000000000 ) ) ;
#4680 = FACE_BOUND ( 'NONE', #8208, .T. ) ;
#4681 = CARTESIAN_POINT ( 'NONE',  ( 5.000000000000000000, -2.000000000000001776, 37.99999999999999289 ) ) ;
#4682 = EDGE_CURVE ( 'NONE', #9602, #12131, #9526, .T. ) ;
#4683 = LINE ( 'NONE', #10984, #16378 ) ;
#4684 = CARTESIAN_POINT ( 'NONE',  ( -3.846120219227901593, 3.114526743279308896, -12.34374999795161543 ) ) ;
#4685 = ORIENTED_EDGE ( 'NONE', *, *, #19313, .F. ) ;
#4686 = FACE_OUTER_BOUND ( 'NONE', #5949, .T. ) ;
#4687 = DIRECTION ( 'NONE',  ( 0.000000000000000000, -1.000000000000000000, 0.000000000000000000 ) ) ;
#4688 = AXIS2_PLACEMENT_3D ( 'NONE', #14400, #17296, #9808 ) ;
#4689 = EDGE_LOOP ( 'NONE', ( #19116, #11764, #16082, #7648 ) ) ;
#4690 = LINE ( 'NONE', #3285, #3684 ) ;
#4692 = EDGE_CURVE ( 'NONE', #10790, #12820, #9211, .T. ) ;
#4691 = EDGE_CURVE ( 'NONE', #2268, #1354, #5047, .T. ) ;
#4693 = CIRCLE ( 'NONE', #211, 5.700000000000001954 ) ;
#4694 = CARTESIAN_POINT ( 'NONE',  ( 17.68117051311639898, -3.372863662543048591, -35.00000000000000000 ) ) ;
#4695 = CARTESIAN_POINT ( 'NONE',  ( -7.937500000000000000, 3.090998114436792843, -0.3168978725525089524 ) ) ;
#4696 = DIRECTION ( 'NONE',  ( 0.000000000000000000, 0.000000000000000000, -1.000000000000000000 ) ) ;
#4697 = ORIENTED_EDGE ( 'NONE', *, *, #6366, .F. ) ;
#4698 = CARTESIAN_POINT ( 'NONE',  ( 7.000000000000005329, 1.761396867937200517, -5.421022142882375938 ) ) ;
#4699 = CARTESIAN_POINT ( 'NONE',  ( -5.209999999999999964, 0.000000000000000000, 0.000000000000000000 ) ) ;
#4700 = CARTESIAN_POINT ( 'NONE',  ( 2.789999999999999147, 20.70663861606293210, -15.04425356660737556 ) ) ;
#4701 = ORIENTED_EDGE ( 'NONE', *, *, #16315, .F. ) ;
#4702 = CARTESIAN_POINT ( 'NONE',  ( 1.734723475976807094E-15, 9.165435523385314198, -0.7089489049740167470 ) ) ;
#4703 = CARTESIAN_POINT ( 'NONE',  ( 12.96874999795161543, -4.150607464521812062, 2.695436003842704764 ) ) ;
#4704 = CARTESIAN_POINT ( 'NONE',  ( 12.50000000000000533, 0.3020334839682475847, 5.763142191869157216 ) ) ;
#4705 = CIRCLE ( 'NONE', #8853, 5.700000000000001954 ) ;
#4706 = DIRECTION ( 'NONE',  ( -1.000000000000000000, -0.000000000000000000, -0.000000000000000000 ) ) ;
#4707 = EDGE_LOOP ( 'NONE', ( #2395, #2145 ) ) ;
#4708 = DIRECTION ( 'NONE',  ( 0.000000000000000000, 0.000000000000000000, 1.000000000000000000 ) ) ;
#4709 = APPLICATION_CONTEXT ( 'automotive_design' ) ;
#4710 = CARTESIAN_POINT ( 'NONE',  ( 0.000000000000000000, 4.484350416777833449E-16, 3.323500000000020993 ) ) ;
#4711 = EDGE_LOOP ( 'NONE', ( #6255, #5433 ) ) ;
#4712 = FACE_OUTER_BOUND ( 'NONE', #2354, .T. ) ;
#4713 = DIRECTION ( 'NONE',  ( 0.000000000000000000, 1.374038396813314756E-15, -1.000000000000000000 ) ) ;
#4714 = ORIENTED_EDGE ( 'NONE', *, *, #5882, .T. ) ;
#4715 = CONTEXT_DEPENDENT_SHAPE_REPRESENTATION ( #18939, #922 ) ;
#4716 = AXIS2_PLACEMENT_3D ( 'NONE', #3098, #15608, #1894 ) ;
#4717 = AXIS2_PLACEMENT_3D ( 'NONE', #18605, #18411, #11006 ) ;
#4718 = CARTESIAN_POINT ( 'NONE',  ( -90.00000000000000000, 0.000000000000000000, -8.073750000000021743 ) ) ;
#4719 = LINE ( 'NONE', #15029, #14493 ) ;
#4720 = ORIENTED_EDGE ( 'NONE', *, *, #10864, .F. ) ;
#4721 = CARTESIAN_POINT ( 'NONE',  ( 4.888101187500000222, -3.413342815706642518E-14, -6.656249997951614539 ) ) ;
#4722 = CARTESIAN_POINT ( 'NONE',  ( 9.468749997951615427, 3.954556930911862000, -2.873153789725825469 ) ) ;
#4723 = ORIENTED_EDGE ( 'NONE', *, *, #18434, .T. ) ;
#4724 = FACE_OUTER_BOUND ( 'NONE', #9165, .T. ) ;
#4725 = ORIENTED_EDGE ( 'NONE', *, *, #18116, .F. ) ;
#4726 = CARTESIAN_POINT ( 'NONE',  ( 2.318398865532038666, -5.207209108562836697, -14.31249999590322552 ) ) ;
#4727 = VERTEX_POINT ( 'NONE', #16726 ) ;
#4728 = CARTESIAN_POINT ( 'NONE',  ( -13.86923836996420967, -11.47363181547641275, -35.00000000000000000 ) ) ;
#4729 = CARTESIAN_POINT ( 'NONE',  ( -1.280903732194487166, -4.780397808154247308, -9.343749997951615427 ) ) ;
#4730 = DIRECTION ( 'NONE',  ( 0.000000000000000000, 0.000000000000000000, 1.000000000000000000 ) ) ;
#4731 = CIRCLE ( 'NONE', #4090, 0.9999999999999974465 ) ;
#4732 = DIRECTION ( 'NONE',  ( 0.000000000000000000, 0.8090169943749527803, -0.5877852522924655876 ) ) ;
#4733 = AXIS2_PLACEMENT_3D ( 'NONE', #12121, #4502, #10619 ) ;
#4734 = EDGE_LOOP ( 'NONE', ( #12024, #15867, #5531, #17461 ) ) ;
#4735 = CARTESIAN_POINT ( 'NONE',  ( 2.999999999999998224, 0.000000000000000000, 0.000000000000000000 ) ) ;
#4736 = EDGE_CURVE ( 'NONE', #2023, #12048, #3004, .T. ) ;
#4737 = ORIENTED_EDGE ( 'NONE', *, *, #13512, .T. ) ;
#4738 = CARTESIAN_POINT ( 'NONE',  ( 1.039999999999994929, -25.12109765559662833, 12.52377138324214023 ) ) ;
#4739 = DIRECTION ( 'NONE',  ( -1.000000000000000000, -0.000000000000000000, -0.000000000000000000 ) ) ;
#4740 = VECTOR ( 'NONE', #11767, 1000.000000000000000 ) ;
#4741 = ORIENTED_EDGE ( 'NONE', *, *, #8685, .F. ) ;
#4742 = CARTESIAN_POINT ( 'NONE',  ( 1.749999999999998002, -27.76164181293054511, 4.147968289691195132 ) ) ;
#4743 = CARTESIAN_POINT ( 'NONE',  ( 14.34374999795161365, 4.780397808154273065, -1.280903732194386802 ) ) ;
#4744 = ORIENTED_EDGE ( 'NONE', *, *, #531, .F. ) ;
#4745 = FACE_OUTER_BOUND ( 'NONE', #10683, .T. ) ;
#4746 = ORIENTED_EDGE ( 'NONE', *, *, #14634, .F. ) ;
#4747 = CONTEXT_DEPENDENT_SHAPE_REPRESENTATION ( #4325, #19280 ) ;
#4748 = CARTESIAN_POINT ( 'NONE',  ( 0.006930995026450970445, 23.92277630352802831, -5.408431875071194384 ) ) ;
#4749 = CARTESIAN_POINT ( 'NONE',  ( 6.000000000000005329, 0.000000000000000000, 0.000000000000000000 ) ) ;
#4750 = VERTEX_POINT ( 'NONE', #17117 ) ;
#4751 = EDGE_CURVE ( 'NONE', #11811, #3123, #9615, .T. ) ;
#4752 = ORIENTED_EDGE ( 'NONE', *, *, #10327, .F. ) ;
#4753 = CARTESIAN_POINT ( 'NONE',  ( -16.28688694438836038, -7.664027248171298545, 32.00000000000000000 ) ) ;
#4754 = CARTESIAN_POINT ( 'NONE',  ( 1.280903732194454081, 4.780397808154257078, -9.343749997951615427 ) ) ;
#4755 = ORIENTED_EDGE ( 'NONE', *, *, #1859, .T. ) ;
#4756 = CIRCLE ( 'NONE', #17547, 4.400000000000000355 ) ;
#4757 = EDGE_CURVE ( 'NONE', #17855, #17528, #11118, .T. ) ;
#4758 = CARTESIAN_POINT ( 'NONE',  ( 2.789999999999999147, -24.34211360614305875, 7.909232158574721616 ) ) ;
#4759 = VERTEX_POINT ( 'NONE', #3604 ) ;
#4760 = PRODUCT_DEFINITION_FORMATION_WITH_SPECIFIED_SOURCE ( 'ANY', '', #8260, .NOT_KNOWN. ) ;
#4761 =( BOUNDED_CURVE ( )  B_SPLINE_CURVE ( 2, ( #3740, #5617, #15851, #8242, #17550, #14348, #11635, #647, #6721, #19045, #12950, #9957, #2235, #5335, #16048, #11539, #17644 ),
 .UNSPECIFIED., .F., .F. ) 
 B_SPLINE_CURVE_WITH_KNOTS ( ( 3, 2, 2, 2, 2, 2, 2, 2, 3 ),
 ( 0.000000000000000000, 0.05000000000000000971, 0.1000000000000000194, 0.1499999999999999944, 0.2000000000000000389, 0.2500000000000000000, 0.2999999999999999889, 0.3499999999999999223, 0.4000000000000000777 ),
 .UNSPECIFIED. ) 
 CURVE ( )  GEOMETRIC_REPRESENTATION_ITEM ( )  RATIONAL_B_SPLINE_CURVE ( ( 1.000000000000000000, 0.9876883405951377704, 1.000000000000000000, 0.9876883405951377704, 1.000000000000000000, 0.9876883405951377704, 1.000000000000000000, 0.9876883405951377704, 1.000000000000000000, 0.9876883405951377704, 1.000000000000000000, 0.9876883405951377704, 1.000000000000000000, 0.9876883405951377704, 1.000000000000000000, 0.9876883405951377704, 1.000000000000000000 ) ) 
 REPRESENTATION_ITEM ( '' )  );
#4762 = B_SPLINE_CURVE_WITH_KNOTS ( 'NONE', 3,
 ( #2105, #17513, #8209, #10943 ),
 .UNSPECIFIED., .F., .F.,
 ( 4, 4 ),
 ( 0.005258110598983628189, 0.005948376585272736536 ),
 .UNSPECIFIED. ) ;
#4763 = CARTESIAN_POINT ( 'NONE',  ( 7.626241948324204323, -16.73597674598852691, -32.00000000000000000 ) ) ;
#4764 = FACE_OUTER_BOUND ( 'NONE', #16120, .T. ) ;
#4765 = CARTESIAN_POINT ( 'NONE',  ( -1.886022603841227552, 0.000000000000000000, -8.265000000000021885 ) ) ;
#4766 = CARTESIAN_POINT ( 'NONE',  ( 2.030753610301984313, -19.12676442129359700, 19.86438386685654578 ) ) ;
#4767 = VECTOR ( 'NONE', #14064, 1000.000000000000000 ) ;
#4768 = ORIENTED_EDGE ( 'NONE', *, *, #7722, .F. ) ;
#4769 = VERTEX_POINT ( 'NONE', #17018 ) ;
#4770 = LINE ( 'NONE', #1574, #18756 ) ;
#4771 = SURFACE_STYLE_FILL_AREA ( #9579 ) ;
#4772 = CARTESIAN_POINT ( 'NONE',  ( 1.800000000000000488, 0.000000000000000000, 0.000000000000000000 ) ) ;
#4773 = EDGE_LOOP ( 'NONE', ( #18932, #11027, #13859, #7229 ) ) ;
#4774 = EDGE_CURVE ( 'NONE', #1756, #1726, #3408, .T. ) ;
#4775 = ORIENTED_EDGE ( 'NONE', *, *, #8444, .T. ) ;
#4776 = DIRECTION ( 'NONE',  ( -1.000000000000000000, -1.224646799147353207E-16, 0.000000000000000000 ) ) ;
#4777 = DIRECTION ( 'NONE',  ( 0.000000000000000000, 1.000000000000000000, 0.000000000000000000 ) ) ;
#4778 = DIRECTION ( 'NONE',  ( 0.000000000000000000, 0.000000000000000000, 1.000000000000000000 ) ) ;
#4779 = DIRECTION ( 'NONE',  ( 0.000000000000000000, 0.000000000000000000, -1.000000000000000000 ) ) ;
#4780 = ADVANCED_FACE ( 'NONE', ( #5095 ), #6486, .F. ) ;
#4781 = CARTESIAN_POINT ( 'NONE',  ( -4.861323657744413218, -0.5109457054261099529, -9.843749997951615427 ) ) ;
#4782 = EDGE_LOOP ( 'NONE', ( #16624, #12568, #13843, #8332 ) ) ;
#4783 = CARTESIAN_POINT ( 'NONE',  ( 2.789999999999999147, -25.59481291497571220, -1.787276233276378314E-13 ) ) ;
#4784 = EDGE_CURVE ( 'NONE', #2358, #15929, #3893, .T. ) ;
#4785 = CARTESIAN_POINT ( 'NONE',  ( 0.02436607992775717893, -9.836394144775869819, 22.71065055754449347 ) ) ;
#4786 = ORIENTED_EDGE ( 'NONE', *, *, #16300, .F. ) ;
#4787 = CARTESIAN_POINT ( 'NONE',  ( 8.500000000000007105, -1.493657965219446382, -5.574407415329178939 ) ) ;
#4788 = FACE_OUTER_BOUND ( 'NONE', #20, .T. ) ;
#4789 = VECTOR ( 'NONE', #9942, 1000.000000000000114 ) ;
#4790 = AXIS2_PLACEMENT_3D ( 'NONE', #17034, #3324, #4011 ) ;
#4791 = DIRECTION ( 'NONE',  ( -0.000000000000000000, -0.000000000000000000, -1.000000000000000000 ) ) ;
#4792 = CARTESIAN_POINT ( 'NONE',  ( 0.1882238946918236844, 2.857713464478689680, 25.78859396478529220 ) ) ;
#4793 = EDGE_CURVE ( 'NONE', #2993, #6802, #18806, .T. ) ;
#4794 = VERTEX_POINT ( 'NONE', #210 ) ;
#4795 = CARTESIAN_POINT ( 'NONE',  ( 2.789999999999999147, 7.772527002114431482, 23.17675759782044054 ) ) ;
#4796 = CARTESIAN_POINT ( 'NONE',  ( 2.789999999999999147, -7.772527002114268058, -23.17675759782048672 ) ) ;
#4797 = DIRECTION ( 'NONE',  ( -1.000000000000000000, -0.000000000000000000, -0.000000000000000000 ) ) ;
#4798 = EDGE_LOOP ( 'NONE', ( #14567, #512, #16554, #435 ) ) ;
#4799 = DIRECTION ( 'NONE',  ( -1.000000000000000000, 1.224646799147353207E-16, 0.000000000000000000 ) ) ;
#4800 = DIRECTION ( 'NONE',  ( -1.000000000000000000, 0.000000000000000000, 0.000000000000000000 ) ) ;
#4801 = EDGE_CURVE ( 'NONE', #303, #18102, #14958, .T. ) ;
#4802 = CARTESIAN_POINT ( 'NONE',  ( 7.468749997951615427, 4.781284448697194378, -1.016293382781411125 ) ) ;
#4803 = ADVANCED_FACE ( 'NONE', ( #17309 ), #12617, .F. ) ;
#4804 = DIRECTION ( 'NONE',  ( -1.000000000000000000, -0.000000000000000000, 0.000000000000000000 ) ) ;
#4805 = EDGE_LOOP ( 'NONE', ( #1529, #9332, #15350, #238, #18701, #12314, #1992, #7348 ) ) ;
#4806 = DIRECTION ( 'NONE',  ( 0.000000000000000000, 0.000000000000000000, -1.000000000000000000 ) ) ;
#4807 = AXIS2_PLACEMENT_3D ( 'NONE', #1896, #13808, #10907 ) ;
#4808 = DIRECTION ( 'NONE',  ( 1.000000000000000000, 6.419766481290786633E-33, -0.000000000000000000 ) ) ;
#4809 = AXIS2_PLACEMENT_3D ( 'NONE', #19089, #2285, #17498 ) ;
#4810 = ORIENTED_EDGE ( 'NONE', *, *, #5582, .T. ) ;
#4811 = DIRECTION ( 'NONE',  ( 0.000000000000000000, 0.000000000000000000, 1.000000000000000000 ) ) ;
#4812 = CARTESIAN_POINT ( 'NONE',  ( 2.765633920072236407, -2.336989772644440855, 24.63872515616082026 ) ) ;
#4813 = ORIENTED_EDGE ( 'NONE', *, *, #11062, .F. ) ;
#4814 = EDGE_CURVE ( 'NONE', #2241, #9243, #6942, .T. ) ;
#4815 = EDGE_CURVE ( 'NONE', #5246, #16591, #5990, .T. ) ;
#4816 = DIRECTION ( 'NONE',  ( -0.000000000000000000, 0.000000000000000000, 1.000000000000000000 ) ) ;
#4817 = EDGE_LOOP ( 'NONE', ( #16060, #3898, #15471, #9741 ) ) ;
#4818 = VECTOR ( 'NONE', #10658, 1000.000000000000000 ) ;
#4819 = CARTESIAN_POINT ( 'NONE',  ( 1.394999999999998685, 24.89775460606851354, -12.96210679857759374 ) ) ;
#4820 = FACE_OUTER_BOUND ( 'NONE', #1045, .T. ) ;
#4821 = ORIENTED_EDGE ( 'NONE', *, *, #11779, .F. ) ;
#4822 = CYLINDRICAL_SURFACE ( 'NONE', #9598, 1.000000000000002665 ) ;
#4823 = ORIENTED_EDGE ( 'NONE', *, *, #10042, .F. ) ;
#4824 = EDGE_CURVE ( 'NONE', #16982, #4071, #17213, .T. ) ;
#4825 = DIRECTION ( 'NONE',  ( 0.000000000000000000, 0.000000000000000000, -1.000000000000000000 ) ) ;
#4826 = ORIENTED_EDGE ( 'NONE', *, *, #16536, .T. ) ;
#4827 = CARTESIAN_POINT ( 'NONE',  ( 1.749999999999998002, -4.633866840649122132, 27.68468304288257542 ) ) ;
#4828 = DIRECTION ( 'NONE',  ( 0.000000000000000000, 0.000000000000000000, 1.000000000000000000 ) ) ;
#4829 = DIRECTION ( 'NONE',  ( 1.000000000000000000, 0.000000000000000000, 0.000000000000000000 ) ) ;
#4830 = ORIENTED_EDGE ( 'NONE', *, *, #3012, .T. ) ;
#4831 = DIRECTION ( 'NONE',  ( 0.4067366430758020401, 0.9135454576426000894, 0.000000000000000000 ) ) ;
#4832 = CIRCLE ( 'NONE', #10270, 1.000000000000000888 ) ;
#4833 = CYLINDRICAL_SURFACE ( 'NONE', #17732, 8.073750000000021743 ) ;
#4834 = AXIS2_PLACEMENT_3D ( 'NONE', #538, #2318, #3918 ) ;
#4835 = ORIENTED_EDGE ( 'NONE', *, *, #429, .T. ) ;
#4836 = EDGE_CURVE ( 'NONE', #3344, #4257, #16925, .T. ) ;
#4837 = CARTESIAN_POINT ( 'NONE',  ( 1.394999999999998685, 12.96210679857822434, -24.89775460606818314 ) ) ;
#4838 = CARTESIAN_POINT ( 'NONE',  ( -1.280903732194487166, -4.780397808154247308, -8.968749997951613651 ) ) ;
#4839 = B_SPLINE_CURVE_WITH_KNOTS ( 'NONE', 3,
 ( #19498, #5988, #18213, #11706 ),
 .UNSPECIFIED., .F., .F.,
 ( 4, 4 ),
 ( 0.005258120783916782857, 0.005948386350302925507 ),
 .UNSPECIFIED. ) ;
#4840 = ORIENTED_EDGE ( 'NONE', *, *, #9198, .F. ) ;
#4841 = CARTESIAN_POINT ( 'NONE',  ( 2.257825491203657275, 11.58891744060141882, -24.44564404695831783 ) ) ;
#4842 = DIRECTION ( 'NONE',  ( 0.000000000000000000, 0.000000000000000000, 1.000000000000000000 ) ) ;
#4843 = ORIENTED_EDGE ( 'NONE', *, *, #17415, .T. ) ;
#4844 = FACE_OUTER_BOUND ( 'NONE', #2817, .T. ) ;
#4845 = TOROIDAL_SURFACE ( 'NONE', #18582, 24.12539914357697768, 8.000000000000000000 ) ;
#4846 = ORIENTED_EDGE ( 'NONE', *, *, #8935, .T. ) ;
#4847 = APPLICATION_PROTOCOL_DEFINITION ( 'draft international standard', 'automotive_design', 1998, #3680 ) ;
#4848 = CIRCLE ( 'NONE', #16039, 2.524999999999996358 ) ;
#4849 = CARTESIAN_POINT ( 'NONE',  ( -0.5958122406256771697, -5.668774803599153422, -8.000000000000005329 ) ) ;
#4850 = EDGE_CURVE ( 'NONE', #676, #19176, #7923, .T. ) ;
#4851 = DIRECTION ( 'NONE',  ( 0.000000000000000000, 0.000000000000000000, 1.000000000000000000 ) ) ;
#4852 = AXIS2_PLACEMENT_3D ( 'NONE', #6196, #9219, #6382 ) ;
#4853 = ORIENTED_EDGE ( 'NONE', *, *, #18375, .F. ) ;
#4854 = EDGE_LOOP ( 'NONE', ( #16505, #8222, #18963, #15871 ) ) ;
#4855 = LINE ( 'NONE', #7754, #924 ) ;
#4856 = CARTESIAN_POINT ( 'NONE',  ( 5.668774803599156975, -0.5958122406256373127, -14.31249999590322552 ) ) ;
#4857 = ORIENTED_EDGE ( 'NONE', *, *, #18421, .F. ) ;
#4858 = EDGE_CURVE ( 'NONE', #12027, #5756, #11022, .T. ) ;
#4859 = CARTESIAN_POINT ( 'NONE',  ( -17.11901729331276911, 5.562305898749051458, -32.00000000000000000 ) ) ;
#4860 = VECTOR ( 'NONE', #15503, 1000.000000000000000 ) ;
#4861 = ORIENTED_EDGE ( 'NONE', *, *, #7903, .T. ) ;
#4862 = AXIS2_PLACEMENT_3D ( 'NONE', #3181, #18297, #18393 ) ;
#4863 = VECTOR ( 'NONE', #17483, 1000.000000000000000 ) ;
#4864 = CARTESIAN_POINT ( 'NONE',  ( 1.749999999999998002, 4.633866840649310426, -27.68468304288254345 ) ) ;
#4865 = VECTOR ( 'NONE', #9909, 1000.000000000000000 ) ;
#4866 = CARTESIAN_POINT ( 'NONE',  ( 7.626241948324204323, -16.73597674598852691, 32.00000000000000000 ) ) ;
#4867 = CARTESIAN_POINT ( 'NONE',  ( -11.58013454126452579, -14.56230589874905235, 35.00000000000000000 ) ) ;
#4868 = ORIENTED_EDGE ( 'NONE', *, *, #14971, .T. ) ;
#4869 = CARTESIAN_POINT ( 'NONE',  ( 2.789999999999999147, 7.909232158575156824, -24.34211360614291664 ) ) ;
#4870 = DIRECTION ( 'NONE',  ( 0.000000000000000000, 0.000000000000000000, 1.000000000000000000 ) ) ;
#4871 = ADVANCED_FACE ( 'NONE', ( #899 ), #5394, .T. ) ;
#4872 = ORIENTED_EDGE ( 'NONE', *, *, #12981, .T. ) ;
#4873 = EDGE_LOOP ( 'NONE', ( #15756, #17891, #6436, #7641 ) ) ;
#4874 = CARTESIAN_POINT ( 'NONE',  ( 4.611396867937200383, 3.350375938067097881, -14.00000000000000533 ) ) ;
#4875 = AXIS2_PLACEMENT_3D ( 'NONE', #1079, #7154, #13280 ) ;
#4876 = CARTESIAN_POINT ( 'NONE',  ( -1.493657965219562511, -5.574407415329147852, -9.812499995903223748 ) ) ;
#4877 = CARTESIAN_POINT ( 'NONE',  ( -5.207209108562804722, 2.318398865532109276, -14.00000000000000533 ) ) ;
#4878 = VECTOR ( 'NONE', #14282, 1000.000000000000000 ) ;
#4879 = DIRECTION ( 'NONE',  ( 1.000000000000000000, 0.000000000000000000, 0.000000000000000000 ) ) ;
#4880 = AXIS2_PLACEMENT_3D ( 'NONE', #4446, #16654, #2934 ) ;
#4881 = CARTESIAN_POINT ( 'NONE',  ( -4.150607464521828938, -2.695436003842674566, -8.343749997951611874 ) ) ;
#4882 = EDGE_LOOP ( 'NONE', ( #16886, #6164, #8380, #7752, #5234 ) ) ;
#4883 = CARTESIAN_POINT ( 'NONE',  ( -13.86923836996420967, -11.47363181547641275, -35.00000000000000000 ) ) ;
#4884 = AXIS2_PLACEMENT_3D ( 'NONE', #8455, #9963, #16056 ) ;
#4885 =( BOUNDED_CURVE ( )  B_SPLINE_CURVE ( 2, ( #3176, #13985, #275, #6357, #4877 ),
 .UNSPECIFIED., .F., .F. ) 
 B_SPLINE_CURVE_WITH_KNOTS ( ( 3, 2, 3 ),
 ( 0.3333180920165860761, 0.3499999999999999778, 0.4000000000000000222 ),
 .UNSPECIFIED. ) 
 CURVE ( )  GEOMETRIC_REPRESENTATION_ITEM ( )  RATIONAL_B_SPLINE_CURVE ( ( 0.9945256517182510247, 0.9958923606136991236, 1.000000000000000000, 0.9876883405951377704, 1.000000000000000000 ) ) 
 REPRESENTATION_ITEM ( '' )  );
#4886 = CARTESIAN_POINT ( 'NONE',  ( 4.476417968967386862, 17.43449690031536292, -32.00000000000000000 ) ) ;
#4887 = ORIENTED_EDGE ( 'NONE', *, *, #4441, .F. ) ;
#4888 = CARTESIAN_POINT ( 'NONE',  ( 12.86923836996420967, -11.47363181547641453, -35.00000000000000000 ) ) ;
#4889 = EDGE_CURVE ( 'NONE', #18915, #16413, #808, .T. ) ;
#4890 = EDGE_CURVE ( 'NONE', #19252, #4244, #3601, .T. ) ;
#4891 = DIRECTION ( 'NONE',  ( 1.000000000000000000, 0.000000000000000000, 0.000000000000000000 ) ) ;
#4892 = CARTESIAN_POINT ( 'NONE',  ( -4.840010801796527318, -3.143139765844555900, -8.812499995903225525 ) ) ;
#4893 = DIRECTION ( 'NONE',  ( -1.000000000000000000, 0.000000000000000000, -0.000000000000000000 ) ) ;
#4894 = CARTESIAN_POINT ( 'NONE',  ( 4.888101187499994893, -0.7741991708319229115, -6.968749997951614539 ) ) ;
#4895 = ORIENTED_EDGE ( 'NONE', *, *, #14470, .T. ) ;
#4896 = AXIS2_PLACEMENT_3D ( 'NONE', #19136, #17640, #932 ) ;
#4897 = DIRECTION ( 'NONE',  ( -0.000000000000000000, 0.000000000000000000, 1.000000000000000000 ) ) ;
#4898 = CARTESIAN_POINT ( 'NONE',  ( 0.000000000000000000, 0.000000000000000000, 0.000000000000000000 ) ) ;
#4899 = EDGE_CURVE ( 'NONE', #15823, #16071, #17260, .T. ) ;
#4900 = COLOUR_RGB ( '', 0.72549020, 0.75294118, 0.79215686) ;
#4901 = CYLINDRICAL_SURFACE ( 'NONE', #974, 28.06981291497571362 ) ;
#4902 = ORIENTED_EDGE ( 'NONE', *, *, #5649, .T. ) ;
#4903 =( NAMED_UNIT ( * ) PLANE_ANGLE_UNIT ( ) SI_UNIT ( $, .RADIAN. ) );
#4904 = DIRECTION ( 'NONE',  ( -1.000000000000000000, -0.000000000000000000, -0.000000000000000000 ) ) ;
#4905 = CARTESIAN_POINT ( 'NONE',  ( -2.000000000000001776, 0.000000000000000000, -6.735000000000022524 ) ) ;
#4906 = ORIENTED_EDGE ( 'NONE', *, *, #8843, .T. ) ;
#4907 = DIRECTION ( 'NONE',  ( 0.000000000000000000, 1.000000000000000000, 0.000000000000000000 ) ) ;
#4908 = CARTESIAN_POINT ( 'NONE',  ( 2.789999999999999147, -7.909232158574647009, -24.34211360614308006 ) ) ;
#4909 = ORIENTED_EDGE ( 'NONE', *, *, #17852, .T. ) ;
#4910 = CARTESIAN_POINT ( 'NONE',  ( 12.00000000000000178, 1.469576158976824144E-15, -30.00000000000000355 ) ) ;
#4911 = DIRECTION ( 'NONE',  ( -0.000000000000000000, -0.000000000000000000, 1.000000000000000000 ) ) ;
#4912 = VERTEX_POINT ( 'NONE', #4095 ) ;
#4913 = AXIS2_PLACEMENT_3D ( 'NONE', #18016, #10411, #13500 ) ;
#4914 = PRODUCT_RELATED_PRODUCT_CATEGORY ( 'part', '', ( #8260 ) ) ;
#4915 = DIRECTION ( 'NONE',  ( 1.000000000000000000, 0.000000000000000000, 0.000000000000000000 ) ) ;
#4916 = CARTESIAN_POINT ( 'NONE',  ( 9.332722423957255486, 2.725425358843983450E-16, 5.700000000000002842 ) ) ;
#4917 = VERTEX_POINT ( 'NONE', #14701 ) ;
#4918 = COLOUR_RGB ( '', 0.31764706, 0.68627451, 0.89019608) ;
#4919 = AXIS2_PLACEMENT_3D ( 'NONE', #11244, #17350, #17549 ) ;
#4920 = CARTESIAN_POINT ( 'NONE',  ( 0.02436607992776064838, 18.55949924794892780, 16.37294372382865504 ) ) ;
#4921 = CARTESIAN_POINT ( 'NONE',  ( -20.63749999999999574, 0.000000000000000000, -7.174999999999998934 ) ) ;
#4922 = ADVANCED_FACE ( 'NONE', ( #5483 ), #11144, .T. ) ;
#4923 = ORIENTED_EDGE ( 'NONE', *, *, #4002, .T. ) ;
#4924 = DIRECTION ( 'NONE',  ( 1.000000000000000000, 0.000000000000000000, 0.000000000000000000 ) ) ;
#4925 = ORIENTED_EDGE ( 'NONE', *, *, #9855, .F. ) ;
#4926 = ADVANCED_FACE ( 'NONE', ( #12096 ), #2777, .T. ) ;
#4927 = FACE_OUTER_BOUND ( 'NONE', #19728, .T. ) ;
#4928 = ORIENTED_EDGE ( 'NONE', *, *, #731, .F. ) ;
#4929 = DIRECTION ( 'NONE',  ( 1.000000000000000000, 0.000000000000000000, 0.000000000000000000 ) ) ;
#4930 = DIRECTION ( 'NONE',  ( -1.000000000000000000, 0.000000000000000000, 0.000000000000000000 ) ) ;
#4931 = FACE_OUTER_BOUND ( 'NONE', #4155, .T. ) ;
#4932 = CARTESIAN_POINT ( 'NONE',  ( 4.861323657744411442, 0.5109457054261445919, -9.843749997951615427 ) ) ;
#4933 = ORIENTED_EDGE ( 'NONE', *, *, #16337, .T. ) ;
#4934 = DIRECTION ( 'NONE',  ( 0.000000000000000000, 0.000000000000000000, -1.000000000000000000 ) ) ;
#4935 = EDGE_CURVE ( 'NONE', #8711, #13634, #18165, .T. ) ;
#4936 = CYLINDRICAL_SURFACE ( 'NONE', #17124, 13.19999999999999929 ) ;
#4937 = AXIS2_PLACEMENT_3D ( 'NONE', #6422, #11639, #19048 ) ;
#4938 = ORIENTED_EDGE ( 'NONE', *, *, #10668, .F. ) ;
#4939 = EDGE_CURVE ( 'NONE', #4625, #16863, #18916, .T. ) ;
#4940 = ORIENTED_EDGE ( 'NONE', *, *, #14097, .F. ) ;
#4941 = EDGE_CURVE ( 'NONE', #2350, #13507, #8675, .T. ) ;
#4942 = AXIS2_PLACEMENT_3D ( 'NONE', #6397, #11026, #15628 ) ;
#4943 = DIRECTION ( 'NONE',  ( -1.000000000000000000, -0.000000000000000000, -0.000000000000000000 ) ) ;
#4944 = DIRECTION ( 'NONE',  ( 0.000000000000000000, 1.000000000000000000, 0.000000000000000000 ) ) ;
#4945 = VERTEX_POINT ( 'NONE', #8991 ) ;
#4946 = CARTESIAN_POINT ( 'NONE',  ( 2.765633920072235519, 9.836394144776026138, -22.71065055754441531 ) ) ;
#4947 = DIRECTION ( 'NONE',  ( 0.000000000000000000, 0.000000000000000000, 1.000000000000000000 ) ) ;
#4948 = ORIENTED_EDGE ( 'NONE', *, *, #7884, .T. ) ;
#4949 = CARTESIAN_POINT ( 'NONE',  ( -41.99999999999999289, 1.999999999999998224, 2.000000000000000000 ) ) ;
#4950 = CIRCLE ( 'NONE', #12308, 2.524999999999995914 ) ;
#4951 = VERTEX_POINT ( 'NONE', #3078 ) ;
#4952 = APPLICATION_PROTOCOL_DEFINITION ( 'draft international standard', 'automotive_design', 1998, #18010 ) ;
#4953 = CARTESIAN_POINT ( 'NONE',  ( 9.332722423957255486, 2.725425358843983450E-16, 5.700000000000002842 ) ) ;
#4954 = CARTESIAN_POINT ( 'NONE',  ( 13.34374999795161365, 0.2590123213420971182, 4.942249507334556924 ) ) ;
#4955 = EDGE_LOOP ( 'NONE', ( #12532, #11050, #5310, #8738, #4031, #13475 ) ) ;
#4956 = EDGE_LOOP ( 'NONE', ( #4902, #11031 ) ) ;
#4957 = CARTESIAN_POINT ( 'NONE',  ( 1.039999999999997815, 27.68468304288265003, -4.633866840648637186 ) ) ;
#4958 = CARTESIAN_POINT ( 'NONE',  ( 13.00000000000000000, -1.727010089215899713, -5.432074755721473025 ) ) ;
#4959 = VERTEX_POINT ( 'NONE', #19780 ) ;
#4960 = EDGE_CURVE ( 'NONE', #15386, #17537, #908, .T. ) ;
#4961 = CARTESIAN_POINT ( 'NONE',  ( 0.5109457054261454800, -4.861323657744410554, -14.84374999795161543 ) ) ;
#4962 = AXIS2_PLACEMENT_3D ( 'NONE', #15987, #2277, #9995 ) ;
#4963 = VERTEX_POINT ( 'NONE', #18199 ) ;
#4964 = B_SPLINE_CURVE_WITH_KNOTS ( 'NONE', 3,
 ( #82, #10887, #6173, #16992, #18198, #12293, #18390, #16896 ),
 .UNSPECIFIED., .F., .F.,
 ( 4, 2, 2, 4 ),
 ( 2.032124546189621919E-07, 0.001631739532304474910, 0.002447507692229407717, 0.003263275852154340524 ),
 .UNSPECIFIED. ) ;
#4965 = DIRECTION ( 'NONE',  ( 0.000000000000000000, 0.000000000000000000, -1.000000000000000000 ) ) ;
#4966 = CARTESIAN_POINT ( 'NONE',  ( 0.000000000000000000, -22.25075486061745167, 9.324097380959385006 ) ) ;
#4967 = DIRECTION ( 'NONE',  ( 0.000000000000000000, 0.000000000000000000, 1.000000000000000000 ) ) ;
#4968 = ORIENTED_EDGE ( 'NONE', *, *, #8826, .T. ) ;
#4969 = DIRECTION ( 'NONE',  ( 0.000000000000000000, 0.000000000000000000, -1.000000000000000000 ) ) ;
#4970 = DIRECTION ( 'NONE',  ( 0.000000000000000000, 0.000000000000000000, 1.000000000000000000 ) ) ;
#4971 = ORIENTED_EDGE ( 'NONE', *, *, #3667, .F. ) ;
#4972 = ORIENTED_EDGE ( 'NONE', *, *, #713, .F. ) ;
#4973 = CARTESIAN_POINT ( 'NONE',  ( 2.765633920072238627, 12.59161484032942901, -21.30679549418617924 ) ) ;
#4974 = TOROIDAL_SURFACE ( 'NONE', #6867, 8.239200000000002078, 0.03079999999999868954 ) ;
#4975 = AXIS2_PLACEMENT_3D ( 'NONE', #2458, #5165, #14494 ) ;
#4976 = DIRECTION ( 'NONE',  ( 0.000000000000000000, 0.000000000000000000, 1.000000000000000000 ) ) ;
#4977 = CARTESIAN_POINT ( 'NONE',  ( -4.484949146646330931, 3.631840208645857437, -12.81249999590322552 ) ) ;
#4978 = ORIENTED_EDGE ( 'NONE', *, *, #4941, .F. ) ;
#4979 = CARTESIAN_POINT ( 'NONE',  ( 22.00000000000000355, 0.000000000000000000, 32.00000000000000000 ) ) ;
#4980 = ORIENTED_EDGE ( 'NONE', *, *, #15753, .F. ) ;
#4981 = DIRECTION ( 'NONE',  ( 1.000000000000000000, 0.000000000000000000, 0.000000000000000000 ) ) ;
#4982 = EDGE_CURVE ( 'NONE', #9521, #9108, #10593, .T. ) ;
#4983 = CARTESIAN_POINT ( 'NONE',  ( 0.7592463896980057303, -19.86438386685674473, 19.12676442129336252 ) ) ;
#4984 = CIRCLE ( 'NONE', #1787, 1.000000000000000888 ) ;
#4985 = CIRCLE ( 'NONE', #8819, 2.524999999999995914 ) ;
#4986 = DIRECTION ( 'NONE',  ( 0.000000000000000000, 0.000000000000000000, -1.000000000000000000 ) ) ;
#4987 = CARTESIAN_POINT ( 'NONE',  ( 1.799999999999999600, 5.021051876504148371E-16, 4.000000000000000000 ) ) ;
#4988 = CARTESIAN_POINT ( 'NONE',  ( 4.611396867937178179, -3.350375938067129855, -8.000000000000005329 ) ) ;
#4989 = EDGE_LOOP ( 'NONE', ( #17391, #1926, #7296, #1259 ) ) ;
#4990 = CARTESIAN_POINT ( 'NONE',  ( 7.500000000000005329, 2.620002426024544029, -5.142044285764750811 ) ) ;
#4991 =( NAMED_UNIT ( * ) SI_UNIT ( $, .STERADIAN. ) SOLID_ANGLE_UNIT ( ) );
#4992 = FACE_OUTER_BOUND ( 'NONE', #15582, .T. ) ;
#4993 = PRESENTATION_STYLE_ASSIGNMENT (( #9509 ) ) ;
#4994 = EDGE_LOOP ( 'NONE', ( #961, #14263 ) ) ;
#4995 = CARTESIAN_POINT ( 'NONE',  ( 8.312499995903225525, 5.575441324182696334, -1.185096637661215535 ) ) ;
#4996 = DIRECTION ( 'NONE',  ( 0.000000000000000000, 0.000000000000000000, -1.000000000000000000 ) ) ;
#4997 = CARTESIAN_POINT ( 'NONE',  ( 0.5958122406255995651, -5.668774803599162304, -14.00000000000000533 ) ) ;
#4998 = CARTESIAN_POINT ( 'NONE',  ( 6.468749997951615427, 4.233219804643871598, 2.444050593750020095 ) ) ;
#4999 = LINE ( 'NONE', #2922, #10832 ) ;
#5000 = EDGE_CURVE ( 'NONE', #8773, #11695, #13788, .T. ) ;
#5001 =( BOUNDED_CURVE ( )  B_SPLINE_CURVE ( 2, ( #8427, #14535, #6899, #13028, #918, #6996, #17720, #19213, #4013, #10124, #13610, #1507, #1305 ),
 .UNSPECIFIED., .F., .F. ) 
 B_SPLINE_CURVE_WITH_KNOTS ( ( 3, 2, 2, 2, 2, 2, 3 ),
 ( 0.000000000000000000, 0.05000000000000000278, 0.1000000000000000056, 0.1499999999999999944, 0.2000000000000000111, 0.2500000000000000000, 0.2843253191101273170 ),
 .UNSPECIFIED. ) 
 CURVE ( )  GEOMETRIC_REPRESENTATION_ITEM ( )  RATIONAL_B_SPLINE_CURVE ( ( 1.000000000000000000, 0.9876883405951377704, 1.000000000000000000, 0.9876883405951377704, 1.000000000000000000, 0.9876883405951377704, 1.000000000000000000, 0.9876883405951377704, 1.000000000000000000, 0.9876883405951377704, 1.000000000000000000, 0.9915479672430580482, 0.9947006833465674713 ) ) 
 REPRESENTATION_ITEM ( '' )  );
#5002 = ORIENTED_EDGE ( 'NONE', *, *, #15249, .T. ) ;
#5003 = CARTESIAN_POINT ( 'NONE',  ( 1.039999999999996927, -4.633866840649124796, 27.68468304288256832 ) ) ;
#5004 = DIRECTION ( 'NONE',  ( 1.000000000000000000, 0.000000000000000000, 0.000000000000000000 ) ) ;
#5005 = VERTEX_POINT ( 'NONE', #11795 ) ;
#5006 = CARTESIAN_POINT ( 'NONE',  ( 12.46874999795161543, -4.648860486681943627, -1.510506337161893642 ) ) ;
#5007 = CARTESIAN_POINT ( 'NONE',  ( 0.000000000000000000, -9.324097380959319281, -22.25075486061748009 ) ) ;
#5008 = ORIENTED_EDGE ( 'NONE', *, *, #1840, .T. ) ;
#5009 = EDGE_CURVE ( 'NONE', #2569, #6283, #10302, .T. ) ;
#5010 = DIRECTION ( 'NONE',  ( 1.000000000000000000, 0.000000000000000000, 0.000000000000000000 ) ) ;
#5011 = CARTESIAN_POINT ( 'NONE',  ( 22.00000000000000355, 0.000000000000000000, 35.00000000000000000 ) ) ;
#5012 = ORIENTED_EDGE ( 'NONE', *, *, #9619, .F. ) ;
#5013 = CARTESIAN_POINT ( 'NONE',  ( 8.671566133830875600, 15.77352024078954784, -32.00000000000000000 ) ) ;
#5014 = LINE ( 'NONE', #15825, #19577 ) ;
#5015 = DIRECTION ( 'NONE',  ( -0.000000000000000000, -0.000000000000000000, -1.000000000000000000 ) ) ;
#5016 = VECTOR ( 'NONE', #5602, 1000.000000000000114 ) ;
#5017 = EDGE_LOOP ( 'NONE', ( #8620, #6425 ) ) ;
#5018 = CARTESIAN_POINT ( 'NONE',  ( 2.789999999999999147, -21.30679549418640306, 12.59161484032904887 ) ) ;
#5019 = ORIENTED_EDGE ( 'NONE', *, *, #8596, .F. ) ;
#5020 = CARTESIAN_POINT ( 'NONE',  ( 3.814044456245474279, -4.235925505221167064, -13.31249999590322730 ) ) ;
#5021 = VERTEX_POINT ( 'NONE', #14996 ) ;
#5022 = CARTESIAN_POINT ( 'NONE',  ( -2.000000000000001776, 3.218695387886217674, -3.000000000000000000 ) ) ;
#5023 = CARTESIAN_POINT ( 'NONE',  ( -4.620319390059841602, -1.773574444220693325, -12.34374999795161543 ) ) ;
#5024 = EDGE_CURVE ( 'NONE', #18274, #19129, #17517, .T. ) ;
#5025 = FACE_OUTER_BOUND ( 'NONE', #9853, .T. ) ;
#5026 = CARTESIAN_POINT ( 'NONE',  ( 4.620319390059819398, -1.773574444220757274, -11.34374999795161543 ) ) ;
#5027 = EDGE_LOOP ( 'NONE', ( #16340, #9939, #15904, #19026 ) ) ;
#5028 = CARTESIAN_POINT ( 'NONE',  ( -20.63749999999999929, 0.000000000000000000, 0.000000000000000000 ) ) ;
#5029 = DIRECTION ( 'NONE',  ( 0.000000000000000000, 0.000000000000000000, 1.000000000000000000 ) ) ;
#5030 = ADVANCED_FACE ( 'NONE', ( #13389 ), #17915, .T. ) ;
#5031 = AXIS2_PLACEMENT_3D ( 'NONE', #19503, #10612, #3495 ) ;
#5032 = ORIENTED_EDGE ( 'NONE', *, *, #13746, .T. ) ;
#5033 = AXIS2_PLACEMENT_3D ( 'NONE', #4242, #949, #11463 ) ;
#5034 = EDGE_CURVE ( 'NONE', #9172, #2365, #12094, .T. ) ;
#5035 = LINE ( 'NONE', #3828, #10957 ) ;
#5036 = DIRECTION ( 'NONE',  ( 0.000000000000000000, 0.000000000000000000, -1.000000000000000000 ) ) ;
#5037 = ORIENTED_EDGE ( 'NONE', *, *, #1023, .F. ) ;
#5038 = CARTESIAN_POINT ( 'NONE',  ( 10.50000000000000533, -3.631840208645763735, -4.484949146646406426 ) ) ;
#5039 = CARTESIAN_POINT ( 'NONE',  ( -41.99999999999999289, 4.999999999999998224, 2.000000000000000000 ) ) ;
#5040 = ORIENTED_EDGE ( 'NONE', *, *, #3900, .F. ) ;
#5041 = ADVANCED_FACE ( 'NONE', ( #8176 ), #15115, .T. ) ;
#5042 = LINE ( 'NONE', #557, #2373 ) ;
#5043 = AXIS2_PLACEMENT_3D ( 'NONE', #18999, #14604, #984 ) ;
#5044 = EDGE_LOOP ( 'NONE', ( #10868, #6394, #19620, #6401 ) ) ;
#5045 = PRODUCT_CONTEXT ( 'NONE', #16226, 'mechanical' ) ;
#5046 = CARTESIAN_POINT ( 'NONE',  ( -4.484949146646406426, -3.631840208645764179, -10.50000000000000711 ) ) ;
#5047 = CIRCLE ( 'NONE', #7590, 2.524999999999997247 ) ;
#5048 = DIRECTION ( 'NONE',  ( -1.000000000000000000, 0.000000000000000000, 0.000000000000000000 ) ) ;
#5049 = ORIENTED_EDGE ( 'NONE', *, *, #16386, .F. ) ;
#5050 = EDGE_LOOP ( 'NONE', ( #16432, #11286 ) ) ;
#5051 = DIRECTION ( 'NONE',  ( 1.000000000000000000, 0.000000000000000000, 0.000000000000000000 ) ) ;
#5052 = CARTESIAN_POINT ( 'NONE',  ( 13.00000000000000178, -0.7793280607714923036, -4.825575716215948496 ) ) ;
#5053 = EDGE_CURVE ( 'NONE', #1430, #8854, #14655, .T. ) ;
#5054 = VERTEX_POINT ( 'NONE', #18881 ) ;
#5055 = FILL_AREA_STYLE ('',( #12767 ) ) ;
#5056 = VECTOR ( 'NONE', #17281, 1000.000000000000000 ) ;
#5057 = ORIENTED_EDGE ( 'NONE', *, *, #7968, .F. ) ;
#5058 = CARTESIAN_POINT ( 'NONE',  ( 2.999999999999998224, 3.218695387886217230, 3.000000000000000000 ) ) ;
#5059 = EDGE_CURVE ( 'NONE', #18433, #4625, #11976, .T. ) ;
#5060 = FACE_OUTER_BOUND ( 'NONE', #2535, .T. ) ;
#5061 = FACE_BOUND ( 'NONE', #14803, .T. ) ;
#5062 = EDGE_LOOP ( 'NONE', ( #16899, #17361, #9935, #14961 ) ) ;
#5063 = CARTESIAN_POINT ( 'NONE',  ( 0.000000000000000000, 0.000000000000000000, 0.000000000000000000 ) ) ;
#5064 =( NAMED_UNIT ( * ) SI_UNIT ( $, .STERADIAN. ) SOLID_ANGLE_UNIT ( ) );
#5065 = ORIENTED_EDGE ( 'NONE', *, *, #19459, .T. ) ;
#5066 = ORIENTED_EDGE ( 'NONE', *, *, #9538, .F. ) ;
#5067 = CARTESIAN_POINT ( 'NONE',  ( -0.5109457054261112852, 4.861323657744413218, -14.46874999795161720 ) ) ;
#5068 = CIRCLE ( 'NONE', #11148, 4.762500000000000178 ) ;
#5069 = DIRECTION ( 'NONE',  ( -1.000000000000000000, -0.000000000000000000, -0.000000000000000000 ) ) ;
#5070 = CARTESIAN_POINT ( 'NONE',  ( -5.700000000000001066, 0.000000000000000000, -6.000000000000005329 ) ) ;
#5071 = PRODUCT_DEFINITION_FORMATION_WITH_SPECIFIED_SOURCE ( 'ANY', '', #17368, .NOT_KNOWN. ) ;
#5072 = ORIENTED_EDGE ( 'NONE', *, *, #8647, .F. ) ;
#5073 = DIRECTION ( 'NONE',  ( -1.000000000000000000, -1.224646799147353207E-16, -0.000000000000000000 ) ) ;
#5074 = DIRECTION ( 'NONE',  ( 0.000000000000000000, 0.000000000000000000, 1.000000000000000000 ) ) ;
#5075 = ORIENTED_EDGE ( 'NONE', *, *, #11034, .T. ) ;
#5076 = CARTESIAN_POINT ( 'NONE',  ( 4.999999999999963585, 7.196152422706642682, 41.99999999999999289 ) ) ;
#5077 = DIRECTION ( 'NONE',  ( -1.000000000000000000, -0.000000000000000000, -0.000000000000000000 ) ) ;
#5078 = AXIS2_PLACEMENT_3D ( 'NONE', #10165, #17569, #3763 ) ;
#5079 = ADVANCED_FACE ( 'NONE', ( #2554 ), #14682, .F. ) ;
#5080 = DIRECTION ( 'NONE',  ( 0.000000000000000000, 0.000000000000000000, -1.000000000000000000 ) ) ;
#5081 = CARTESIAN_POINT ( 'NONE',  ( 0.006931054464085539824, -24.42321038836781355, -2.248820353273226491 ) ) ;
#5082 = CARTESIAN_POINT ( 'NONE',  ( 5.700000000000002842, 2.725425358843983450E-16, -9.332722423957255486 ) ) ;
#5083 = CARTESIAN_POINT ( 'NONE',  ( -10.00000000000000000, 0.000000000000000000, 0.000000000000000000 ) ) ;
#5084 = SHAPE_REPRESENTATION_RELATIONSHIP ( 'NONE' , 'NONE' ,  #2588, #19745 ) ;
#5085 = CARTESIAN_POINT ( 'NONE',  ( 0.000000000000000000, 9.184850993605147944E-16, -7.500000000000000000 ) ) ;
#5086 = ORIENTED_EDGE ( 'NONE', *, *, #14648, .F. ) ;
#5087 = DIRECTION ( 'NONE',  ( -1.000000000000000000, -0.000000000000000000, -0.000000000000000000 ) ) ;
#5088 = DIRECTION ( 'NONE',  ( 1.000000000000000000, 4.163336342344335449E-15, -0.000000000000000000 ) ) ;
#5089 = CARTESIAN_POINT ( 'NONE',  ( 0.000000000000000000, -12.52067188844364587, 20.62201879784910119 ) ) ;
#5090 = EDGE_CURVE ( 'NONE', #18458, #9357, #19110, .T. ) ;
#5091 = CARTESIAN_POINT ( 'NONE',  ( 2.500000000000000888, 0.000000000000000000, -6.200000000000021494 ) ) ;
#5092 = CARTESIAN_POINT ( 'NONE',  ( 0.5958122406255995651, -5.668774803599162304, -14.00000000000000533 ) ) ;
#5093 = ORIENTED_EDGE ( 'NONE', *, *, #17146, .T. ) ;
#5094 = CARTESIAN_POINT ( 'NONE',  ( -4.999999999999966249, -7.196152422706654228, 41.99999999999999289 ) ) ;
#5095 = FACE_OUTER_BOUND ( 'NONE', #15594, .T. ) ;
#5096 = ORIENTED_EDGE ( 'NONE', *, *, #197, .F. ) ;
#5097 = DIRECTION ( 'NONE',  ( 1.000000000000000000, 0.000000000000000000, 0.000000000000000000 ) ) ;
#5098 = AXIS2_PLACEMENT_3D ( 'NONE', #10127, #8524, #2410 ) ;
#5099 = ORIENTED_EDGE ( 'NONE', *, *, #10121, .T. ) ;
#5100 = EDGE_CURVE ( 'NONE', #13272, #9559, #8804, .T. ) ;
#5101 = DIRECTION ( 'NONE',  ( 1.000000000000000000, 6.419766481290786633E-33, -0.000000000000000000 ) ) ;
#5102 = CARTESIAN_POINT ( 'NONE',  ( 11.00000000000000711, -2.850000000000023626, 4.936344801571289409 ) ) ;
#5103 = ORIENTED_EDGE ( 'NONE', *, *, #11112, .F. ) ;
#5104 = DIRECTION ( 'NONE',  ( 0.000000000000000000, 0.3090169943749544457, -0.9510565162951513107 ) ) ;
#5105 = DIRECTION ( 'NONE',  ( -1.000000000000000000, 0.000000000000000000, 0.000000000000000000 ) ) ;
#5106 = ORIENTED_EDGE ( 'NONE', *, *, #13821, .T. ) ;
#5107 = CARTESIAN_POINT ( 'NONE',  ( 9.968749997951617203, -4.409619785863921670, 2.246813503491803310 ) ) ;
#5108 = ORIENTED_EDGE ( 'NONE', *, *, #18398, .F. ) ;
#5109 =( BOUNDED_CURVE ( )  B_SPLINE_CURVE ( 2, ( #18344, #4634, #6218, #16645, #10646, #12345, #4341, #1538, #15349, #13740, #15445, #1631, #3028, #2926, #1736 ),
 .UNSPECIFIED., .F., .F. ) 
 B_SPLINE_CURVE_WITH_KNOTS ( ( 3, 2, 2, 2, 2, 2, 2, 3 ),
 ( 0.000000000000000000, 0.05000000000000000971, 0.1000000000000000194, 0.1499999999999999944, 0.2000000000000000389, 0.2500000000000000000, 0.2999999999999999889, 0.3265529187307102399 ),
 .UNSPECIFIED. ) 
 CURVE ( )  GEOMETRIC_REPRESENTATION_ITEM ( )  RATIONAL_B_SPLINE_CURVE ( ( 1.000000000000000000, 0.9876883405951377704, 1.000000000000000000, 0.9876883405951377704, 1.000000000000000000, 0.9876883405951377704, 1.000000000000000000, 0.9876883405951377704, 1.000000000000000000, 0.9876883405951377704, 1.000000000000000000, 0.9876883405951377704, 1.000000000000000000, 0.9934617901676501273, 0.9938679225082089896 ) ) 
 REPRESENTATION_ITEM ( '' )  );
#5110 = DIRECTION ( 'NONE',  ( -1.000000000000000000, -0.000000000000000000, -0.000000000000000000 ) ) ;
#5111 = ORIENTED_EDGE ( 'NONE', *, *, #13538, .F. ) ;
#5112 = AXIS2_PLACEMENT_3D ( 'NONE', #12802, #8402, #8198 ) ;
#5113 = AXIS2_PLACEMENT_3D ( 'NONE', #2019, #125, #13930 ) ;
#5114 = CARTESIAN_POINT ( 'NONE',  ( 2.262072625383133140, -4.996265754456554298, 26.57710921259759829 ) ) ;
#5115 = EDGE_CURVE ( 'NONE', #16011, #8576, #2272, .T. ) ;
#5116 = CARTESIAN_POINT ( 'NONE',  ( 1.039999999999995373, 12.96210679857822434, -24.89775460606817958 ) ) ;
#5117 = CARTESIAN_POINT ( 'NONE',  ( 2.765633920072234631, 16.37294372382885044, -18.55949924794875017 ) ) ;
#5118 = CARTESIAN_POINT ( 'NONE',  ( 14.86923836996420434, -11.47363181547641453, -32.00000000000000000 ) ) ;
#5119 = EDGE_LOOP ( 'NONE', ( #11179, #13248, #11514, #13307 ) ) ;
#5120 = DIRECTION ( 'NONE',  ( 0.000000000000000000, 0.000000000000000000, 1.000000000000000000 ) ) ;
#5121 = CARTESIAN_POINT ( 'NONE',  ( -11.00000000000000355, -4.215373648918918192, 3.375000000000000888 ) ) ;
#5122 = ORIENTED_EDGE ( 'NONE', *, *, #9921, .F. ) ;
#5123 = AXIS2_PLACEMENT_3D ( 'NONE', #191, #6563, #287 ) ;
#5124 = CARTESIAN_POINT ( 'NONE',  ( -3.000000000000002665, 0.000000000000000000, 0.000000000000000000 ) ) ;
#5125 = MECHANICAL_DESIGN_GEOMETRIC_PRESENTATION_REPRESENTATION (  '', ( #9616 ), #17920 ) ;
#5126 = CARTESIAN_POINT ( 'NONE',  ( 6.626241948324199882, -16.73597674598852691, -35.00000000000000000 ) ) ;
#5127 = EDGE_CURVE ( 'NONE', #10762, #11999, #8571, .T. ) ;
#5128 = CARTESIAN_POINT ( 'NONE',  ( -4.620319390059842490, -1.773574444220693325, -11.96874999795161365 ) ) ;
#5129 = ORIENTED_EDGE ( 'NONE', *, *, #10628, .F. ) ;
#5130 = FACE_OUTER_BOUND ( 'NONE', #776, .T. ) ;
#5131 = FACE_OUTER_BOUND ( 'NONE', #7335, .T. ) ;
#5132 = CARTESIAN_POINT ( 'NONE',  ( 10.34374999795161543, -0.2590123213421313686, 4.942249507334556036 ) ) ;
#5133 = EDGE_LOOP ( 'NONE', ( #8441, #9065, #2718, #15843 ) ) ;
#5134 = DIRECTION ( 'NONE',  ( 0.000000000000000000, 0.000000000000000000, -1.000000000000000000 ) ) ;
#5135 = EDGE_CURVE ( 'NONE', #10068, #3527, #2088, .T. ) ;
#5136 = ORIENTED_EDGE ( 'NONE', *, *, #10236, .F. ) ;
#5137 = CARTESIAN_POINT ( 'NONE',  ( 10.34374999795161543, -0.2590123213421313686, 4.942249507334556036 ) ) ;
#5138 = DIRECTION ( 'NONE',  ( -1.000000000000000000, 0.000000000000000000, 0.000000000000000000 ) ) ;
#5139 = ORIENTED_EDGE ( 'NONE', *, *, #465, .F. ) ;
#5140 = VERTEX_POINT ( 'NONE', #781 ) ;
#5141 = DIRECTION ( 'NONE',  ( 1.000000000000000000, 0.000000000000000000, 0.000000000000000000 ) ) ;
#5142 = CARTESIAN_POINT ( 'NONE',  ( 1.394999999999999574, -20.02152543075359858, 19.67366047555523778 ) ) ;
#5143 = VECTOR ( 'NONE', #12552, 1000.000000000000000 ) ;
#5144 = DIRECTION ( 'NONE',  ( -1.000000000000000000, -0.000000000000000000, -0.000000000000000000 ) ) ;
#5145 = ORIENTED_EDGE ( 'NONE', *, *, #5009, .F. ) ;
#5146 = SURFACE_SIDE_STYLE ('',( #766 ) ) ;
#5147 = ORIENTED_EDGE ( 'NONE', *, *, #13235, .T. ) ;
#5148 = CIRCLE ( 'NONE', #5786, 1.000000000000000888 ) ;
#5149 = AXIS2_PLACEMENT_3D ( 'NONE', #15420, #18418, #1903 ) ;
#5150 = CARTESIAN_POINT ( 'NONE',  ( -5.575441324182703440, -1.185096637661177343, -12.00000000000000533 ) ) ;
#5151 = CONICAL_SURFACE ( 'NONE', #3876, 4.000000000000000000, 0.7853981633974458365 ) ;
#5152 = DIRECTION ( 'NONE',  ( 0.000000000000000000, 0.000000000000000000, -1.000000000000000000 ) ) ;
#5153 = FACE_BOUND ( 'NONE', #6399, .T. ) ;
#5154 = VERTEX_POINT ( 'NONE', #11573 ) ;
#5156 = DIRECTION ( 'NONE',  ( -1.000000000000000000, -0.000000000000000000, -0.000000000000000000 ) ) ;
#5155 = B_SPLINE_CURVE_WITH_KNOTS ( 'NONE', 3,
 ( #10368, #9259, #13657, #6041 ),
 .UNSPECIFIED., .F., .F.,
 ( 4, 4 ),
 ( 1.981826382900847025E-07, 0.0006887856082032273912 ),
 .UNSPECIFIED. ) ;
#5157 = SURFACE_SIDE_STYLE ('',( #4771 ) ) ;
#5158 = CARTESIAN_POINT ( 'NONE',  ( 3.270778111535338262, 3.632567103900523620, -10.46874999795161720 ) ) ;
#5159 = EDGE_CURVE ( 'NONE', #6823, #15675, #13641, .T. ) ;
#5160 = ORIENTED_EDGE ( 'NONE', *, *, #1632, .T. ) ;
#5161 = VERTEX_POINT ( 'NONE', #16279 ) ;
#5162 = EDGE_CURVE ( 'NONE', #13659, #12561, #6554, .T. ) ;
#5163 = CARTESIAN_POINT ( 'NONE',  ( 2.444050593750020095, 4.233219804643871598, -6.843749997951615427 ) ) ;
#5164 = AXIS2_PLACEMENT_3D ( 'NONE', #6591, #3316, #5010 ) ;
#5165 = DIRECTION ( 'NONE',  ( 0.000000000000000000, 0.000000000000000000, 1.000000000000000000 ) ) ;
#5166 = CIRCLE ( 'NONE', #15092, 1.000000000000002665 ) ;
#5167 = ORIENTED_EDGE ( 'NONE', *, *, #6998, .F. ) ;
#5168 = ADVANCED_FACE ( 'NONE', ( #5561 ), #12883, .F. ) ;
#5169 = LINE ( 'NONE', #11185, #3587 ) ;
#5170 = AXIS2_PLACEMENT_3D ( 'NONE', #18831, #11339, #8127 ) ;
#5171 = DIRECTION ( 'NONE',  ( -0.000000000000000000, -0.000000000000000000, 1.000000000000000000 ) ) ;
#5172 = VERTEX_POINT ( 'NONE', #11671 ) ;
#5173 = DIRECTION ( 'NONE',  ( 0.000000000000000000, 0.000000000000000000, 1.000000000000000000 ) ) ;
#5174 = CARTESIAN_POINT ( 'NONE',  ( 2.789999999999999147, 24.04302995059966364, 1.991882183130384121 ) ) ;
#5175 = EDGE_CURVE ( 'NONE', #11476, #3823, #11371, .T. ) ;
#5176 = ADVANCED_FACE ( 'NONE', ( #6657, #3673 ), #11285, .T. ) ;
#5177 = CARTESIAN_POINT ( 'NONE',  ( -2.000000000000001776, 0.000000000000000000, 0.000000000000000000 ) ) ;
#5178 = CARTESIAN_POINT ( 'NONE',  ( 0.02436607992776021470, 21.30679549418649543, -12.59161484032888723 ) ) ;
#5179 = LINE ( 'NONE', #11298, #18657 ) ;
#5180 = AXIS2_PLACEMENT_3D ( 'NONE', #3877, #19084, #11583 ) ;
#5181 = DIRECTION ( 'NONE',  ( -1.000000000000000000, -0.000000000000000000, -0.000000000000000000 ) ) ;
#5182 = SURFACE_STYLE_USAGE ( .BOTH. , #500 ) ;
#5183 = CYLINDRICAL_SURFACE ( 'NONE', #7071, 5.700000000000001954 ) ;
#5184 = CIRCLE ( 'NONE', #15426, 1.000000000000002665 ) ;
#5185 = CARTESIAN_POINT ( 'NONE',  ( -9.671566133830877376, 15.77352024078954429, 32.00000000000000000 ) ) ;
#5186 = EDGE_LOOP ( 'NONE', ( #16500, #5213, #7235, #4300 ) ) ;
#5187 = DIRECTION ( 'NONE',  ( 0.000000000000000000, 0.000000000000000000, 1.000000000000000000 ) ) ;
#5188 = CARTESIAN_POINT ( 'NONE',  ( -0.000000000000000000, 0.000000000000000000, 0.000000000000000000 ) ) ;
#5189 = LINE ( 'NONE', #11307, #10570 ) ;
#5190 = AXIS2_PLACEMENT_3D ( 'NONE', #5437, #14257, #12956 ) ;
#5191 = CARTESIAN_POINT ( 'NONE',  ( 12.32184790671639618, 13.12143529358541016, -32.00000000000000000 ) ) ;
#5192 = CARTESIAN_POINT ( 'NONE',  ( 7.343749997951615427, -4.620319390059841602, 1.773574444220693103 ) ) ;
#5193 = ORIENTED_EDGE ( 'NONE', *, *, #10518, .T. ) ;
#5194 = CYLINDRICAL_SURFACE ( 'NONE', #14475, 2.524999999999995914 ) ;
#5195 = DIRECTION ( 'NONE',  ( 0.000000000000000000, 0.000000000000000000, -1.000000000000000000 ) ) ;
#5196 = ORIENTED_EDGE ( 'NONE', *, *, #13088, .T. ) ;
#5197 = CARTESIAN_POINT ( 'NONE',  ( 7.312499995903225525, -3.980288726281172656E-14, 5.700000000000001066 ) ) ;
#5198 = EDGE_CURVE ( 'NONE', #16569, #16271, #15839, .T. ) ;
#5199 = CARTESIAN_POINT ( 'NONE',  ( 0.07181523211952839381, -10.24584646439522828, -23.19431517146944088 ) ) ;
#5200 = VECTOR ( 'NONE', #8561, 1000.000000000000000 ) ;
#5201 = ORIENTED_EDGE ( 'NONE', *, *, #17761, .F. ) ;
#5202 = LINE ( 'NONE', #9826, #9428 ) ;
#5203 = DIRECTION ( 'NONE',  ( 0.000000000000000000, 0.000000000000000000, -1.000000000000000000 ) ) ;
#5204 = EDGE_CURVE ( 'NONE', #1899, #2597, #32, .T. ) ;
#5205 = AXIS2_PLACEMENT_3D ( 'NONE', #16859, #6133, #5935 ) ;
#5206 = EDGE_CURVE ( 'NONE', #2023, #13547, #12329, .T. ) ;
#5207 = AXIS2_PLACEMENT_3D ( 'NONE', #14894, #1184, #19001 ) ;
#5208 = CARTESIAN_POINT ( 'NONE',  ( 2.604434404052932805, -19.17825124759790256, 17.45907811351449368 ) ) ;
#5209 = CARTESIAN_POINT ( 'NONE',  ( 13.00000000000000533, -5.207209108562836697, 2.318398865532038666 ) ) ;
#5210 = ORIENTED_EDGE ( 'NONE', *, *, #1555, .F. ) ;
#5211 = LINE ( 'NONE', #17619, #3720 ) ;
#5212 = CARTESIAN_POINT ( 'NONE',  ( 1.039999999999997593, 0.000000000000000000, 0.000000000000000000 ) ) ;
#5213 = ORIENTED_EDGE ( 'NONE', *, *, #13583, .T. ) ;
#5214 = DIRECTION ( 'NONE',  ( 1.000000000000000000, 0.000000000000000000, 0.000000000000000000 ) ) ;
#5215 = ORIENTED_EDGE ( 'NONE', *, *, #3586, .T. ) ;
#5216 = CARTESIAN_POINT ( 'NONE',  ( -30.00000000000000000, 1.224646799147352468E-16, 0.000000000000000000 ) ) ;
#5217 = ORIENTED_EDGE ( 'NONE', *, *, #456, .T. ) ;
#5218 = EDGE_CURVE ( 'NONE', #1741, #1756, #9140, .T. ) ;
#5219 = CARTESIAN_POINT ( 'NONE',  ( -3.889375000000000693, 4.763110644433737781E-16, -0.6113687067993561763 ) ) ;
#5220 = CARTESIAN_POINT ( 'NONE',  ( -3.490243377569957047E-16, 5.700000000000001066, -12.31249999590322552 ) ) ;
#5221 = PRODUCT ( 'CLUTCH CONE', 'CLUTCH CONE', '', ( #9463 ) ) ;
#5222 = LINE ( 'NONE', #9641, #15720 ) ;
#5223 = CYLINDRICAL_SURFACE ( 'NONE', #8250, 4.000000000000000000 ) ;
#5224 = ORIENTED_EDGE ( 'NONE', *, *, #3655, .T. ) ;
#5225 = AXIS2_PLACEMENT_3D ( 'NONE', #12918, #4104, #17615 ) ;
#5226 = DIRECTION ( 'NONE',  ( 1.000000000000000000, 0.000000000000000000, -0.000000000000000000 ) ) ;
#5227 = DIRECTION ( 'NONE',  ( 0.000000000000000000, 0.000000000000000000, 1.000000000000000000 ) ) ;
#5228 = ORIENTED_EDGE ( 'NONE', *, *, #2168, .T. ) ;
#5229 =( GEOMETRIC_REPRESENTATION_CONTEXT ( 3 ) GLOBAL_UNCERTAINTY_ASSIGNED_CONTEXT ( ( #11990 ) ) GLOBAL_UNIT_ASSIGNED_CONTEXT ( ( #18020, #4303, #7688 ) ) REPRESENTATION_CONTEXT ( 'NONE', 'WORKASPACE' ) );
#5230 = CARTESIAN_POINT ( 'NONE',  ( -36.00000000000000000, -2.311115933264683024E-31, 0.000000000000000000 ) ) ;
#5231 = ADVANCED_FACE ( 'NONE', ( #4465 ), #14775, .T. ) ;
#5232 = CARTESIAN_POINT ( 'NONE',  ( 5.626241948324195441, -16.73597674598852691, -32.00000000000000000 ) ) ;
#5233 = CARTESIAN_POINT ( 'NONE',  ( -3.270778111535363131, -3.632567103900500971, -10.46874999795161720 ) ) ;
#5234 = ORIENTED_EDGE ( 'NONE', *, *, #6140, .F. ) ;
#5235 = CARTESIAN_POINT ( 'NONE',  ( -4.611396867937224364, -3.350375938067065906, -14.00000000000000533 ) ) ;
#5236 = FACE_OUTER_BOUND ( 'NONE', #19658, .T. ) ;
#5237 = CLOSED_SHELL ( 'NONE', ( #14485, #3217, #14989, #4250, #14217, #18580, #18570, #13866, #10815, #9582, #12509, #19633, #16393, #11700, #8046, #1640, #2589, #16211, #17219, #3177, #492, #1097, #6247, #19199, #8587, #11, #2471, #17465 ) ) ;
#5238 = CIRCLE ( 'NONE', #18034, 7.174999999999998934 ) ;
#5239 = ORIENTED_EDGE ( 'NONE', *, *, #2480, .T. ) ;
#5240 = CYLINDRICAL_SURFACE ( 'NONE', #13557, 1.000000000000002665 ) ;
#5241 = B_SPLINE_CURVE_WITH_KNOTS ( 'NONE', 3,
 ( #605, #7043, #19265, #19363 ),
 .UNSPECIFIED., .F., .F.,
 ( 4, 4 ),
 ( 0.005258105385878670927, 0.005948373736081390140 ),
 .UNSPECIFIED. ) ;
#5242 = VERTEX_POINT ( 'NONE', #5658 ) ;
#5243 = ITEM_DEFINED_TRANSFORMATION ( 'NONE', 'NONE', #7942,  #16724 ) ;
#5244 = CARTESIAN_POINT ( 'NONE',  ( 18.68117051311639543, -3.372863662543048591, 32.00000000000000000 ) ) ;
#5245 = ORIENTED_EDGE ( 'NONE', *, *, #7855, .T. ) ;
#5246 = VERTEX_POINT ( 'NONE', #14874 ) ;
#5247 = CARTESIAN_POINT ( 'NONE',  ( 3.499494075959791672, -3.499494075959840966, -9.343749997951615427 ) ) ;
#5248 = CARTESIAN_POINT ( 'NONE',  ( 9.332722423957255486, 2.725425358843983450E-16, 5.700000000000002842 ) ) ;
#5249 = CARTESIAN_POINT ( 'NONE',  ( 17.68117051311639898, -3.372863662543048591, 32.00000000000000000 ) ) ;
#5250 = ORIENTED_EDGE ( 'NONE', *, *, #18777, .T. ) ;
#5251 = B_SPLINE_CURVE_WITH_KNOTS ( 'NONE', 3,
 ( #7450, #4272, #16581, #15076, #14879, #4371 ),
 .UNSPECIFIED., .F., .F.,
 ( 4, 2, 4 ),
 ( 2.032124546189808531E-07, 0.001878594002992309232, 0.003756984793529999193 ),
 .UNSPECIFIED. ) ;
#5252 = EDGE_CURVE ( 'NONE', #1773, #1219, #7671, .T. ) ;
#5253 = CARTESIAN_POINT ( 'NONE',  ( -3.632567103900569361, -3.270778111535287191, -7.843749997951614539 ) ) ;
#5254 = TOROIDAL_SURFACE ( 'NONE', #16443, 8.239200000000002078, 0.03079999999999868954 ) ;
#5255 = ORIENTED_EDGE ( 'NONE', *, *, #9270, .T. ) ;
#5256 = EDGE_CURVE ( 'NONE', #8384, #639, #7517, .T. ) ;
#5257 = AXIS2_PLACEMENT_3D ( 'NONE', #16951, #16557, #10746 ) ;
#5258 = CARTESIAN_POINT ( 'NONE',  ( -15.00000000000000355, 8.000000000000000000, 0.000000000000000000 ) ) ;
#5259 = DIRECTION ( 'NONE',  ( -0.000000000000000000, 0.000000000000000000, 1.000000000000000000 ) ) ;
#5260 = CARTESIAN_POINT ( 'NONE',  ( -2.255998204157477538, -17.85806462366060288, -32.00000000000000000 ) ) ;
#5261 = EDGE_LOOP ( 'NONE', ( #15884, #7933 ) ) ;
#5262 = DIRECTION ( 'NONE',  ( 0.000000000000000000, 0.000000000000000000, 1.000000000000000000 ) ) ;
#5263 = SURFACE_STYLE_USAGE ( .BOTH. , #5360 ) ;
#5264 = DIRECTION ( 'NONE',  ( 0.000000000000000000, 0.000000000000000000, -1.000000000000000000 ) ) ;
#5265 = AXIS2_PLACEMENT_3D ( 'NONE', #15011, #2892, #7380 ) ;
#5266 = EDGE_LOOP ( 'NONE', ( #13863, #18635, #119, #5476, #13025, #15939 ) ) ;
#5267 = VERTEX_POINT ( 'NONE', #16374 ) ;
#5268 = DIRECTION ( 'NONE',  ( 0.000000000000000000, -1.000000000000000000, 0.000000000000000000 ) ) ;
#5269 = ADVANCED_FACE ( 'NONE', ( #2755 ), #19762, .F. ) ;
#5270 = DIRECTION ( 'NONE',  ( 0.000000000000000000, 0.000000000000000000, 1.000000000000000000 ) ) ;
#5271 = AXIS2_PLACEMENT_3D ( 'NONE', #7876, #3387, #15595 ) ;
#5272 = DIRECTION ( 'NONE',  ( -1.000000000000000000, -0.000000000000000000, -0.000000000000000000 ) ) ;
#5273 = ORIENTED_EDGE ( 'NONE', *, *, #3062, .F. ) ;
#5274 = CARTESIAN_POINT ( 'NONE',  ( -41.99999999999999289, -5.000000000000001776, 2.000000000000000000 ) ) ;
#5275 = B_SPLINE_CURVE_WITH_KNOTS ( 'NONE', 3,
 ( #2769, #8885, #7357, #19581 ),
 .UNSPECIFIED., .F., .F.,
 ( 4, 4 ),
 ( 2.324263106244697256E-07, 0.0006888201370294697295 ),
 .UNSPECIFIED. ) ;
#5276 = FACE_OUTER_BOUND ( 'NONE', #2813, .T. ) ;
#5277 = ORIENTED_EDGE ( 'NONE', *, *, #15502, .T. ) ;
#5278 = LINE ( 'NONE', #17489, #18385 ) ;
#5279 = EDGE_CURVE ( 'NONE', #6013, #15601, #2725, .T. ) ;
#5280 = EDGE_CURVE ( 'NONE', #17299, #15369, #12004, .T. ) ;
#5281 = CARTESIAN_POINT ( 'NONE',  ( 12.00000000000000533, 5.421022142882376826, 1.761396867937200073 ) ) ;
#5282 = CARTESIAN_POINT ( 'NONE',  ( 1.039999999999996705, -20.02152543075331081, -19.67366047555552555 ) ) ;
#5283 = DIRECTION ( 'NONE',  ( -1.000000000000000000, -0.000000000000000000, -0.000000000000000000 ) ) ;
#5284 = CARTESIAN_POINT ( 'NONE',  ( 5.421022142882364392, -1.761396867937238486, -7.000000000000005329 ) ) ;
#5285 = AXIS2_PLACEMENT_3D ( 'NONE', #12059, #15554, #18646 ) ;
#5286 = CARTESIAN_POINT ( 'NONE',  ( 1.899999999999999023, 0.000000000000000000, 0.000000000000000000 ) ) ;
#5287 =( LENGTH_UNIT ( ) NAMED_UNIT ( * ) SI_UNIT ( .MILLI., .METRE. ) );
#5288 = CARTESIAN_POINT ( 'NONE',  ( -2.000000000000001776, 8.786840783882259896E-16, 7.175000000000000711 ) ) ;
#5289 = VECTOR ( 'NONE', #12940, 1000.000000000000000 ) ;
#5290 = CARTESIAN_POINT ( 'NONE',  ( -2.068159791354183596, 5.387740456496234565, -7.812499995903224637 ) ) ;
#5291 = VERTEX_POINT ( 'NONE', #2957 ) ;
#5292 = ADVANCED_FACE ( 'NONE', ( #7146 ), #7242, .F. ) ;
#5293 = CARTESIAN_POINT ( 'NONE',  ( 2.789999999999999147, 23.31896751603331808, 7.334849878007589474 ) ) ;
#5294 = DIRECTION ( 'NONE',  ( 0.000000000000000000, 0.000000000000000000, 1.000000000000000000 ) ) ;
#5295 = CARTESIAN_POINT ( 'NONE',  ( 2.850000000000024070, 4.936344801571289409, -7.312499995903225525 ) ) ;
#5296 = CARTESIAN_POINT ( 'NONE',  ( 12.34374999795161543, -1.773574444220693325, -4.620319390059841602 ) ) ;
#5297 = DIRECTION ( 'NONE',  ( -0.9945218953682746221, -0.1045284632676418413, 0.000000000000000000 ) ) ;
#5298 = CARTESIAN_POINT ( 'NONE',  ( -3.846120219227966430, -3.114526743279228072, -11.34374999795161543 ) ) ;
#5300 = ADVANCED_FACE ( 'NONE', ( #13366 ), #5954, .T. ) ;
#5299 = EDGE_CURVE ( 'NONE', #4071, #10940, #3379, .T. ) ;
#5301 = ORIENTED_EDGE ( 'NONE', *, *, #13494, .T. ) ;
#5302 = CARTESIAN_POINT ( 'NONE',  ( 7.812499995903224637, -0.9027913098498965283, 5.699999999999994849 ) ) ;
#5303 = CARTESIAN_POINT ( 'NONE',  ( 5.574407415329170057, 1.493657965219485018, -9.812499995903225525 ) ) ;
#5304 = AXIS2_PLACEMENT_3D ( 'NONE', #15952, #9862, #3836 ) ;
#5305 = VERTEX_POINT ( 'NONE', #18076 ) ;
#5306 = AXIS2_PLACEMENT_3D ( 'NONE', #13621, #10429, #13919 ) ;
#5307 = LINE ( 'NONE', #6792, #10579 ) ;
#5308 = FACE_OUTER_BOUND ( 'NONE', #14019, .T. ) ;
#5309 = CARTESIAN_POINT ( 'NONE',  ( -3.954556930911881096, -2.873153789725797935, -14.84374999795161543 ) ) ;
#5310 = ORIENTED_EDGE ( 'NONE', *, *, #4026, .F. ) ;
#5311 = CARTESIAN_POINT ( 'NONE',  ( 16.11901729331276556, 5.562305898749055011, -32.00000000000000000 ) ) ;
#5312 = CARTESIAN_POINT ( 'NONE',  ( 4.150607464521811174, 2.695436003842704764, -8.343749997951613651 ) ) ;
#5313 = VERTEX_POINT ( 'NONE', #10477 ) ;
#5314 = CARTESIAN_POINT ( 'NONE',  ( 0.02436607992775978102, -12.59161484032896361, -21.30679549418645280 ) ) ;
#5315 = ORIENTED_EDGE ( 'NONE', *, *, #14959, .F. ) ;
#5316 = DIRECTION ( 'NONE',  ( 1.000000000000000000, 0.000000000000000000, 0.000000000000000000 ) ) ;
#5317 = AXIS2_PLACEMENT_3D ( 'NONE', #2617, #6112, #8731 ) ;
#5318 = ORIENTED_EDGE ( 'NONE', *, *, #6103, .T. ) ;
#5319 = CARTESIAN_POINT ( 'NONE',  ( 0.7589665089996477931, -12.05173163741739906, 24.80232951178374279 ) ) ;
#5320 = AXIS2_PLACEMENT_3D ( 'NONE', #10891, #14286, #9292 ) ;
#5321 = LINE ( 'NONE', #17532, #5016 ) ;
#5322 = DIRECTION ( 'NONE',  ( 0.000000000000000000, 0.000000000000000000, 1.000000000000000000 ) ) ;
#5323 = CARTESIAN_POINT ( 'NONE',  ( -5.421022142882375938, 1.761396867937200517, -7.000000000000005329 ) ) ;
#5324 = ORIENTED_EDGE ( 'NONE', *, *, #13442, .F. ) ;
#5325 = FACE_BOUND ( 'NONE', #11568, .T. ) ;
#5326 = CYLINDRICAL_SURFACE ( 'NONE', #5607, 0.9999999999999974465 ) ;
#5327 = VERTEX_POINT ( 'NONE', #2857 ) ;
#5328 = AXIS2_PLACEMENT_3D ( 'NONE', #390, #9209, #15311 ) ;
#5329 = DIRECTION ( 'NONE',  ( -1.000000000000000000, 0.000000000000000000, 0.000000000000000000 ) ) ;
#5330 = AXIS2_PLACEMENT_3D ( 'NONE', #1604, #6578, #205 ) ;
#5331 = DIRECTION ( 'NONE',  ( 0.000000000000000000, 0.000000000000000000, 1.000000000000000000 ) ) ;
#5332 = CARTESIAN_POINT ( 'NONE',  ( -3.350375938067128967, -4.611396867937178179, -14.31249999590322552 ) ) ;
#5333 = ORIENTED_EDGE ( 'NONE', *, *, #18231, .F. ) ;
#5334 = CARTESIAN_POINT ( 'NONE',  ( 0.07186814640506890284, 21.92302674874982316, -12.74240566898960303 ) ) ;
#5335 = CARTESIAN_POINT ( 'NONE',  ( -2.246813503491864150, -4.409619785863891472, -12.96874999795161543 ) ) ;
#5336 = CARTESIAN_POINT ( 'NONE',  ( 13.00000000000000178, -0.5876048313370498821, -4.852654302691288279 ) ) ;
#5337 = ORIENTED_EDGE ( 'NONE', *, *, #3702, .T. ) ;
#5338 = CARTESIAN_POINT ( 'NONE',  ( 0.07186811453410731076, 16.91241718342026346, -18.89333555428536826 ) ) ;
#5339 = ORIENTED_EDGE ( 'NONE', *, *, #8678, .T. ) ;
#5340 = CARTESIAN_POINT ( 'NONE',  ( -11.32184790671638730, 13.12143529358541549, -32.00000000000000000 ) ) ;
#5341 = CYLINDRICAL_SURFACE ( 'NONE', #8674, 4.400000000000000355 ) ;
#5342 = ORIENTED_EDGE ( 'NONE', *, *, #1443, .T. ) ;
#5343 = ORIENTED_EDGE ( 'NONE', *, *, #17045, .T. ) ;
#5344 = CARTESIAN_POINT ( 'NONE',  ( 2.873153789725797491, -3.954556930911881985, -9.843749997951615427 ) ) ;
#5345 = DIRECTION ( 'NONE',  ( 0.000000000000000000, 0.000000000000000000, 1.000000000000000000 ) ) ;
#5346 = CONICAL_SURFACE ( 'NONE', #2449, 3.593999999999999861, 0.2132412839022289897 ) ;
#5347 = CYLINDRICAL_SURFACE ( 'NONE', #12067, 7.174999999999998934 ) ;
#5348 = EDGE_CURVE ( 'NONE', #2770, #11430, #3688, .T. ) ;
#5349 = AXIS2_PLACEMENT_3D ( 'NONE', #11163, #763, #18658 ) ;
#5350 = EDGE_LOOP ( 'NONE', ( #9294, #13605, #16354, #11965 ) ) ;
#5351 = CARTESIAN_POINT ( 'NONE',  ( -90.00000000000000000, 8.247996192257451316E-16, 6.735000000000022524 ) ) ;
#5352 = ORIENTED_EDGE ( 'NONE', *, *, #12479, .T. ) ;
#5353 = AXIS2_PLACEMENT_3D ( 'NONE', #15730, #3326, #12339 ) ;
#5354 = CARTESIAN_POINT ( 'NONE',  ( -15.28688694438835505, -7.664027248171298545, -32.00000000000000000 ) ) ;
#5355 = VECTOR ( 'NONE', #19715, 1000.000000000000000 ) ;
#5356 = DIRECTION ( 'NONE',  ( 1.000000000000000000, 6.419766481290786633E-33, -0.000000000000000000 ) ) ;
#5358 = EDGE_CURVE ( 'NONE', #10744, #725, #5923, .T. ) ;
#5357 = ORIENTED_EDGE ( 'NONE', *, *, #12753, .F. ) ;
#5359 = CARTESIAN_POINT ( 'NONE',  ( -1.280903732194386802, 4.780397808154273065, -14.34374999795161365 ) ) ;
#5360 = SURFACE_SIDE_STYLE ('',( #18972 ) ) ;
#5361 = CARTESIAN_POINT ( 'NONE',  ( -1.016293382781411125, 4.781284448697194378, -7.468749997951615427 ) ) ;
#5362 = VERTEX_POINT ( 'NONE', #2225 ) ;
#5363 = VERTEX_POINT ( 'NONE', #14338 ) ;
#5364 = CARTESIAN_POINT ( 'NONE',  ( -3.632567103900569361, -3.270778111535287191, -7.468749997951615427 ) ) ;
#5365 = EDGE_CURVE ( 'NONE', #9369, #13000, #13922, .T. ) ;
#5366 = CARTESIAN_POINT ( 'NONE',  ( 2.789999999999999147, -5.535312321042889394, 23.48180575137727999 ) ) ;
#5367 = CARTESIAN_POINT ( 'NONE',  ( 0.5321745379877897975, -12.96514671151783915, 23.74442027961355706 ) ) ;
#5368 = VECTOR ( 'NONE', #14611, 1000.000000000000114 ) ;
#5369 = ORIENTED_EDGE ( 'NONE', *, *, #9301, .F. ) ;
#5370 = CARTESIAN_POINT ( 'NONE',  ( 13.84374999795161543, 4.465502636338051445, -1.988169868018530906 ) ) ;
#5371 = CARTESIAN_POINT ( 'NONE',  ( -5.209999999999999964, 0.000000000000000000, 0.000000000000000000 ) ) ;
#5372 = ORIENTED_EDGE ( 'NONE', *, *, #10549, .F. ) ;
#5373 = LINE ( 'NONE', #3678, #1449 ) ;
#5374 = DIRECTION ( 'NONE',  ( 1.000000000000000000, 0.000000000000000000, 0.000000000000000000 ) ) ;
#5375 = CARTESIAN_POINT ( 'NONE',  ( 0.009068833172775131110, 21.10834851580723992, -12.54305517365597922 ) ) ;
#5376 = ADVANCED_FACE ( 'NONE', ( #17340 ), #4936, .T. ) ;
#5377 = CARTESIAN_POINT ( 'NONE',  ( 11.34374999795161543, -3.114526743279228072, -3.846120219227966430 ) ) ;
#5378 = PRODUCT_DEFINITION_SHAPE ( 'NONE', 'NONE',  #19790 ) ;
#5379 = ADVANCED_FACE ( 'NONE', ( #17239 ), #9645, .F. ) ;
#5380 = DIRECTION ( 'NONE',  ( 3.873737557103174326E-15, -1.000000000000000000, 0.000000000000000000 ) ) ;
#5381 =( NAMED_UNIT ( * ) SI_UNIT ( $, .STERADIAN. ) SOLID_ANGLE_UNIT ( ) );
#5382 = FACE_OUTER_BOUND ( 'NONE', #53, .T. ) ;
#5383 = DIRECTION ( 'NONE',  ( 0.9340060080012955179, 4.375140065418144668E-17, 0.3572572980604928339 ) ) ;
#5384 = ORIENTED_EDGE ( 'NONE', *, *, #18760, .T. ) ;
#5385 = CARTESIAN_POINT ( 'NONE',  ( 4.476417968967386862, 17.43449690031536292, 32.00000000000000000 ) ) ;
#5386 = EDGE_CURVE ( 'NONE', #15383, #17455, #17444, .T. ) ;
#5387 = CARTESIAN_POINT ( 'NONE',  ( 17.28688694438834972, -7.664027248171309203, 35.00000000000000000 ) ) ;
#5388 = UNCERTAINTY_MEASURE_WITH_UNIT (LENGTH_MEASURE( 1.000000000000000082E-05 ), #9778, 'distance_accuracy_value', 'NONE');
#5389 = DIRECTION ( 'NONE',  ( 0.000000000000000000, 0.000000000000000000, 1.000000000000000000 ) ) ;
#5390 =( GEOMETRIC_REPRESENTATION_CONTEXT ( 3 ) GLOBAL_UNCERTAINTY_ASSIGNED_CONTEXT ( ( #10399 ) ) GLOBAL_UNIT_ASSIGNED_CONTEXT ( ( #8268, #2450, #3861 ) ) REPRESENTATION_CONTEXT ( 'NONE', 'WORKASPACE' ) );
#5391 = LINE ( 'NONE', #3891, #8926 ) ;
#5392 = EDGE_CURVE ( 'NONE', #18565, #14953, #17440, .T. ) ;
#5393 = DIRECTION ( 'NONE',  ( 0.000000000000000000, 1.000000000000000000, 0.000000000000000000 ) ) ;
#5394 = CYLINDRICAL_SURFACE ( 'NONE', #11456, 13.19999999999999574 ) ;
#5395 = VERTEX_POINT ( 'NONE', #14440 ) ;
#5396 = CARTESIAN_POINT ( 'NONE',  ( 11.34374999795161543, -4.888101187500005551, 0.7741991708318548548 ) ) ;
#5397 = DIRECTION ( 'NONE',  ( 0.000000000000000000, 0.000000000000000000, 1.000000000000000000 ) ) ;
#5398 = AXIS2_PLACEMENT_3D ( 'NONE', #460, #8254, #17259 ) ;
#5399 = VERTEX_POINT ( 'NONE', #2031 ) ;
#5400 = FILL_AREA_STYLE_COLOUR ( '', #8776 ) ;
#5401 = ADVANCED_FACE ( 'NONE', ( #14137 ), #5326, .F. ) ;
#5402 = CARTESIAN_POINT ( 'NONE',  ( 0.000000000000000000, 0.000000000000000000, 0.000000000000000000 ) ) ;
#5403 = DIRECTION ( 'NONE',  ( -1.000000000000000000, -0.000000000000000000, -0.000000000000000000 ) ) ;
#5404 = CYLINDRICAL_SURFACE ( 'NONE', #7449, 28.06981291497571362 ) ;
#5405 = ORIENTED_EDGE ( 'NONE', *, *, #8309, .F. ) ;
#5406 = DIRECTION ( 'NONE',  ( 0.000000000000000000, 0.000000000000000000, -1.000000000000000000 ) ) ;
#5407 = EDGE_CURVE ( 'NONE', #6719, #18587, #14240, .T. ) ;
#5408 = CARTESIAN_POINT ( 'NONE',  ( 2.789999999999999147, 23.17675759782041212, -7.772527002114516748 ) ) ;
#5409 = LINE ( 'NONE', #14533, #1609 ) ;
#5410 = EDGE_LOOP ( 'NONE', ( #17654, #16795 ) ) ;
#5411 = CARTESIAN_POINT ( 'NONE',  ( -36.00000000000000000, 4.200000000000000178, 5.143516556418882928E-16 ) ) ;
#5412 = ORIENTED_EDGE ( 'NONE', *, *, #1397, .F. ) ;
#5413 = CARTESIAN_POINT ( 'NONE',  ( -2.624330855611205937, 7.650277397455539585, -0.08160424337824208341 ) ) ;
#5414 = CARTESIAN_POINT ( 'NONE',  ( 2.604434514863827488, 23.63475234378997314, -10.67816411292140444 ) ) ;
#5415 = DIRECTION ( 'NONE',  ( -0.000000000000000000, -0.000000000000000000, 1.000000000000000000 ) ) ;
#5416 = VECTOR ( 'NONE', #18050, 1000.000000000000000 ) ;
#5417 = CARTESIAN_POINT ( 'NONE',  ( -12.00000000000000178, 0.000000000000000000, -30.00000000000000355 ) ) ;
#5418 = VERTEX_POINT ( 'NONE', #11439 ) ;
#5419 = FACE_BOUND ( 'NONE', #7383, .T. ) ;
#5420 = DIRECTION ( 'NONE',  ( 0.000000000000000000, 0.000000000000000000, 1.000000000000000000 ) ) ;
#5421 = EDGE_LOOP ( 'NONE', ( #13302, #6886, #10808, #3540 ) ) ;
#5422 = EDGE_CURVE ( 'NONE', #18804, #8859, #2106, .T. ) ;
#5423 = DIRECTION ( 'NONE',  ( -1.000000000000000000, 0.000000000000000000, 0.000000000000000000 ) ) ;
#5424 = CARTESIAN_POINT ( 'NONE',  ( 0.7741991708318548548, -4.888101187500005551, -11.34374999795161543 ) ) ;
#5425 = EDGE_CURVE ( 'NONE', #1354, #18489, #1141, .T. ) ;
#5426 = EDGE_LOOP ( 'NONE', ( #2013, #10250, #10231, #13046 ) ) ;
#5428 = CARTESIAN_POINT ( 'NONE',  ( 1.869199999999999973, 0.000000000000000000, 0.000000000000000000 ) ) ;
#5427 = AXIS2_PLACEMENT_3D ( 'NONE', #7918, #8124, #229 ) ;
#5429 = CARTESIAN_POINT ( 'NONE',  ( -0.9027913098498963063, -5.699999999999994849, -11.50000000000000355 ) ) ;
#5430 = EDGE_CURVE ( 'NONE', #16213, #4447, #18078, .T. ) ;
#5431 = CIRCLE ( 'NONE', #19170, 7.174999999999999822 ) ;
#5432 = CARTESIAN_POINT ( 'NONE',  ( -8.776855558857221240, 3.635492607468361115, 0.000000000000000000 ) ) ;
#5433 = ORIENTED_EDGE ( 'NONE', *, *, #18434, .F. ) ;
#5434 = DIRECTION ( 'NONE',  ( -0.000000000000000000, -0.000000000000000000, 1.000000000000000000 ) ) ;
#5435 = ORIENTED_EDGE ( 'NONE', *, *, #14453, .T. ) ;
#5436 = ITEM_DEFINED_TRANSFORMATION ( 'NONE', 'NONE', #1250,  #16724 ) ;
#5437 = CARTESIAN_POINT ( 'NONE',  ( -36.00000000000000000, -2.311115933264683024E-31, 0.000000000000000000 ) ) ;
#5438 = DIRECTION ( 'NONE',  ( 0.000000000000000000, 0.000000000000000000, -1.000000000000000000 ) ) ;
#5439 = DIRECTION ( 'NONE',  ( 1.000000000000000000, 0.000000000000000000, 0.000000000000000000 ) ) ;
#5440 = ORIENTED_EDGE ( 'NONE', *, *, #11529, .F. ) ;
#5441 = DIRECTION ( 'NONE',  ( 1.000000000000000000, 0.000000000000000000, 0.000000000000000000 ) ) ;
#5442 = CARTESIAN_POINT ( 'NONE',  ( 8.000000000000005329, 2.318398865532038666, 5.207209108562838473 ) ) ;
#5443 = DIRECTION ( 'NONE',  ( -1.000000000000000000, -1.224646799147353207E-16, 0.000000000000000000 ) ) ;
#5444 = ORIENTED_EDGE ( 'NONE', *, *, #14201, .T. ) ;
#5445 = CIRCLE ( 'NONE', #16629, 4.000000000000000000 ) ;
#5446 = MECHANICAL_DESIGN_GEOMETRIC_PRESENTATION_REPRESENTATION (  '', ( #15990 ), #7964 ) ;
#5447 = CARTESIAN_POINT ( 'NONE',  ( 50.00050000000000239, 0.000000000000000000, 0.000000000000000000 ) ) ;
#5448 = EDGE_CURVE ( 'NONE', #1013, #6790, #3855, .T. ) ;
#5449 = EDGE_LOOP ( 'NONE', ( #13982, #3168, #10333, #2840 ) ) ;
#5450 = DIRECTION ( 'NONE',  ( 1.000000000000000000, 0.000000000000000000, 0.000000000000000000 ) ) ;
#5451 = EDGE_CURVE ( 'NONE', #11752, #813, #18733, .T. ) ;
#5452 = B_SPLINE_CURVE_WITH_KNOTS ( 'NONE', 3,
 ( #12987, #13277, #11675, #15985, #10090, #16282, #9798, #878, #6764, #11387 ),
 .UNSPECIFIED., .F., .F.,
 ( 4, 3, 3, 4 ),
 ( 0.000000000000000000, 0.0001875345074742618286, 0.0003808595644229699983, 0.0005744879655065563686 ),
 .UNSPECIFIED. ) ;
#5453 = DIRECTION ( 'NONE',  ( -0.000000000000000000, -0.000000000000000000, 1.000000000000000000 ) ) ;
#5454 = ORIENTED_EDGE ( 'NONE', *, *, #14648, .T. ) ;
#5455 = CARTESIAN_POINT ( 'NONE',  ( -3.846120219227901593, 3.114526743279308896, -12.34374999795161543 ) ) ;
#5456 = ORIENTED_EDGE ( 'NONE', *, *, #15321, .T. ) ;
#5457 = ORIENTED_EDGE ( 'NONE', *, *, #8478, .T. ) ;
#5458 = CARTESIAN_POINT ( 'NONE',  ( -2.695436003842674566, 4.150607464521828938, -12.96874999795161543 ) ) ;
#5459 = EDGE_CURVE ( 'NONE', #2358, #16588, #18639, .T. ) ;
#5460 = DIRECTION ( 'NONE',  ( 0.000000000000000000, 0.000000000000000000, -1.000000000000000000 ) ) ;
#5461 = CARTESIAN_POINT ( 'NONE',  ( 1.493657965219523875, 5.574407415329157622, -8.500000000000005329 ) ) ;
#5462 = VERTEX_POINT ( 'NONE', #17143 ) ;
#5463 = DIRECTION ( 'NONE',  ( 1.000000000000000000, 0.000000000000000000, 0.000000000000000000 ) ) ;
#5464 = CARTESIAN_POINT ( 'NONE',  ( 7.312499995903225525, 4.936344801571308061, -2.849999999999989431 ) ) ;
#5465 = AXIS2_PLACEMENT_3D ( 'NONE', #690, #6768, #15896 ) ;
#5466 = ORIENTED_EDGE ( 'NONE', *, *, #10417, .F. ) ;
#5467 = CARTESIAN_POINT ( 'NONE',  ( 2.789999999999999147, -1.991882183130126549, -24.04302995059967429 ) ) ;
#5468 = VECTOR ( 'NONE', #4343, 1000.000000000000000 ) ;
#5469 = VECTOR ( 'NONE', #11839, 1000.000000000000000 ) ;
#5470 = EDGE_CURVE ( 'NONE', #3033, #2077, #13285, .T. ) ;
#5471 = CARTESIAN_POINT ( 'NONE',  ( 2.604434514863827488, -10.67816411292148793, -23.63475234378993761 ) ) ;
#5472 = CYLINDRICAL_SURFACE ( 'NONE', #4595, 4.400000000000000355 ) ;
#5473 = CARTESIAN_POINT ( 'NONE',  ( 9.343749997951615427, -4.780397808154247308, -1.280903732194487166 ) ) ;
#5474 = CARTESIAN_POINT ( 'NONE',  ( 9.812499995903225525, 1.493657965219485018, 5.574407415329170057 ) ) ;
#5475 = DIRECTION ( 'NONE',  ( 0.000000000000000000, 0.000000000000000000, -1.000000000000000000 ) ) ;
#5476 = ORIENTED_EDGE ( 'NONE', *, *, #2405, .F. ) ;
#5477 = DIRECTION ( 'NONE',  ( 1.000000000000000000, 0.000000000000000000, 0.000000000000000000 ) ) ;
#5478 = AXIS2_PLACEMENT_3D ( 'NONE', #14736, #14930, #6918 ) ;
#5479 = CARTESIAN_POINT ( 'NONE',  ( -4.465502636338010589, 1.988169868018623720, -14.84374999795161543 ) ) ;
#5480 = CIRCLE ( 'NONE', #13161, 1.000000000000002665 ) ;
#5481 = PLANE ( 'NONE',  #6077 ) ;
#5482 = CARTESIAN_POINT ( 'NONE',  ( 1.300631254478300303, -8.414515718495838570, -0.3148715423363500632 ) ) ;
#5483 = FACE_OUTER_BOUND ( 'NONE', #7418, .T. ) ;
#5484 = EDGE_CURVE ( 'NONE', #15829, #10318, #4648, .T. ) ;
#5485 = VERTEX_POINT ( 'NONE', #6611 ) ;
#5486 = CARTESIAN_POINT ( 'NONE',  ( 12.81249999590322552, -5.699999999999994849, -0.9027913098498961952 ) ) ;
#5487 = VECTOR ( 'NONE', #4578, 1000.000000000000000 ) ;
#5488 = EDGE_CURVE ( 'NONE', #3927, #2850, #18389, .T. ) ;
#5489 = EDGE_CURVE ( 'NONE', #19760, #11964, #14876, .T. ) ;
#5490 = LINE ( 'NONE', #13206, #2752 ) ;
#5491 = ORIENTED_EDGE ( 'NONE', *, *, #19459, .F. ) ;
#5492 = CARTESIAN_POINT ( 'NONE',  ( 2.999999999999998224, 0.000000000000000000, 0.000000000000000000 ) ) ;
#5493 = CARTESIAN_POINT ( 'NONE',  ( -5.700000000000001066, 0.000000000000000000, -7.312499995903225525 ) ) ;
#5494 = VECTOR ( 'NONE', #6082, 1000.000000000000000 ) ;
#5495 = AXIS2_PLACEMENT_3D ( 'NONE', #16190, #13276, #11773 ) ;
#5496 = EDGE_CURVE ( 'NONE', #11752, #530, #16145, .T. ) ;
#5497 = AXIS2_PLACEMENT_3D ( 'NONE', #8300, #5297, #19006 ) ;
#5498 = FACE_OUTER_BOUND ( 'NONE', #19520, .T. ) ;
#5499 = CARTESIAN_POINT ( 'NONE',  ( 1.886022603841296608, 0.000000000000000000, -6.735000000000022524 ) ) ;
#5500 = ORIENTED_EDGE ( 'NONE', *, *, #18232, .T. ) ;
#5501 = FACE_BOUND ( 'NONE', #12681, .T. ) ;
#5502 = FACE_OUTER_BOUND ( 'NONE', #4873, .T. ) ;
#5503 = AXIS2_PLACEMENT_3D ( 'NONE', #12778, #2164, #11277 ) ;
#5504 = CARTESIAN_POINT ( 'NONE',  ( 13.00000000000000533, -0.5958122406256377568, 5.668774803599156975 ) ) ;
#5505 = ORIENTED_EDGE ( 'NONE', *, *, #8932, .F. ) ;
#5506 = DIRECTION ( 'NONE',  ( 1.000000000000000000, 0.000000000000000000, 0.000000000000000000 ) ) ;
#5507 = ORIENTED_EDGE ( 'NONE', *, *, #17312, .F. ) ;
#5508 = DIRECTION ( 'NONE',  ( 0.000000000000000000, 0.000000000000000000, 1.000000000000000000 ) ) ;
#5509 = FACE_OUTER_BOUND ( 'NONE', #4504, .T. ) ;
#5510 = DIRECTION ( 'NONE',  ( -1.000000000000000000, 0.000000000000000000, -0.000000000000000000 ) ) ;
#5511 = VECTOR ( 'NONE', #15379, 1000.000000000000000 ) ;
#5512 = FACE_OUTER_BOUND ( 'NONE', #7410, .T. ) ;
#5513 = ORIENTED_EDGE ( 'NONE', *, *, #9678, .T. ) ;
#5514 = AXIS2_PLACEMENT_3D ( 'NONE', #15940, #2223, #10134 ) ;
#5515 = CARTESIAN_POINT ( 'NONE',  ( -1.381028087215756681E-16, 24.22479935914660132, 2.133490293297101381 ) ) ;
#5516 = CARTESIAN_POINT ( 'NONE',  ( 0.000000000000000000, 0.000000000000000000, -30.00000000000000355 ) ) ;
#5517 = EDGE_LOOP ( 'NONE', ( #12064, #12264 ) ) ;
#5518 = VECTOR ( 'NONE', #1839, 1000.000000000000000 ) ;
#5519 =( BOUNDED_CURVE ( )  B_SPLINE_CURVE ( 2, ( #18505, #7795, #11101, #12505, #16823 ),
 .UNSPECIFIED., .F., .F. ) 
 B_SPLINE_CURVE_WITH_KNOTS ( ( 3, 2, 3 ),
 ( 0.3333180920165871863, 0.3499999999999999778, 0.4000000000000000222 ),
 .UNSPECIFIED. ) 
 CURVE ( )  GEOMETRIC_REPRESENTATION_ITEM ( )  RATIONAL_B_SPLINE_CURVE ( ( 0.9945256517182510247, 0.9958923606136993456, 1.000000000000000000, 0.9876883405951377704, 1.000000000000000000 ) ) 
 REPRESENTATION_ITEM ( '' )  );
#5520 = EDGE_CURVE ( 'NONE', #18200, #3546, #15869, .T. ) ;
#5521 = CARTESIAN_POINT ( 'NONE',  ( 6.656249997951614539, 4.233219804643871598, 2.444050593750020095 ) ) ;
#5522 = CARTESIAN_POINT ( 'NONE',  ( -41.99999999999999289, -5.000000000000001776, 5.000000000000000000 ) ) ;
#5523 = EDGE_CURVE ( 'NONE', #17548, #4589, #2418, .T. ) ;
#5524 = VERTEX_POINT ( 'NONE', #8531 ) ;
#5525 = CONICAL_SURFACE ( 'NONE', #10967, 7.937500000000000000, 1.047197551196596521 ) ;
#5526 = CARTESIAN_POINT ( 'NONE',  ( -7.937499999999998224, -3.837375845242624095, -0.4937872269236123768 ) ) ;
#5527 = CARTESIAN_POINT ( 'NONE',  ( -3.945386292505473391E-14, -5.700000000000001066, -11.00000000000000711 ) ) ;
#5528 = CARTESIAN_POINT ( 'NONE',  ( 6.468749997951615427, 0.000000000000000000, -4.888101187500000222 ) ) ;
#5529 = VERTEX_POINT ( 'NONE', #10233 ) ;
#5530 = DIRECTION ( 'NONE',  ( 1.000000000000000000, 0.000000000000000000, 0.000000000000000000 ) ) ;
#5531 = ORIENTED_EDGE ( 'NONE', *, *, #17001, .T. ) ;
#5532 = DIRECTION ( 'NONE',  ( 1.000000000000000000, 0.000000000000000000, 0.000000000000000000 ) ) ;
#5533 = LINE ( 'NONE', #2627, #2264 ) ;
#5534 = AXIS2_PLACEMENT_3D ( 'NONE', #11790, #2673, #8590 ) ;
#5535 = FACE_OUTER_BOUND ( 'NONE', #107, .T. ) ;
#5536 = ORIENTED_EDGE ( 'NONE', *, *, #883, .F. ) ;
#5537 = EDGE_CURVE ( 'NONE', #17114, #8958, #12342, .T. ) ;
#5538 = DIRECTION ( 'NONE',  ( -0.7071067811865492381, 8.659560562354910671E-17, -0.7071067811865457964 ) ) ;
#5539 = DIRECTION ( 'NONE',  ( 0.000000000000000000, 0.000000000000000000, 1.000000000000000000 ) ) ;
#5540 = CARTESIAN_POINT ( 'NONE',  ( -11.00000000000000355, -4.898587196589412829E-16, 0.000000000000000000 ) ) ;
#5541 = ORIENTED_EDGE ( 'NONE', *, *, #16918, .T. ) ;
#5542 = EDGE_CURVE ( 'NONE', #488, #736, #8622, .T. ) ;
#5543 = EDGE_CURVE ( 'NONE', #1207, #3249, #5933, .T. ) ;
#5544 = DIRECTION ( 'NONE',  ( 0.000000000000000000, 0.000000000000000000, 1.000000000000000000 ) ) ;
#5545 = ORIENTED_EDGE ( 'NONE', *, *, #6637, .F. ) ;
#5546 = CONICAL_SURFACE ( 'NONE', #19271, 4.762500000000000178, 0.9599310885968813656 ) ;
#5547 = LINE ( 'NONE', #4056, #14039 ) ;
#5548 = CARTESIAN_POINT ( 'NONE',  ( 6.500000000000005329, -0.9027913098498966393, 5.699999999999994849 ) ) ;
#5549 = VERTEX_POINT ( 'NONE', #13415 ) ;
#5550 = CARTESIAN_POINT ( 'NONE',  ( -10.00000000000000000, 0.000000000000000000, 0.000000000000000000 ) ) ;
#5551 = MECHANICAL_DESIGN_GEOMETRIC_PRESENTATION_REPRESENTATION (  '', ( #16753 ), #17699 ) ;
#5552 = CIRCLE ( 'NONE', #10678, 2.524999999999994582 ) ;
#5553 = ADVANCED_FACE ( 'NONE', ( #16431 ), #4024, .F. ) ;
#5554 = VERTEX_POINT ( 'NONE', #19318 ) ;
#5555 = ORIENTED_EDGE ( 'NONE', *, *, #17208, .F. ) ;
#5556 = CARTESIAN_POINT ( 'NONE',  ( -6.929096493834647319, 2.870125742738179664, 12.00000000000000000 ) ) ;
#5557 = CARTESIAN_POINT ( 'NONE',  ( 13.32184790671640151, 13.12143529358541016, -35.00000000000000000 ) ) ;
#5559 = ORIENTED_EDGE ( 'NONE', *, *, #11628, .T. ) ;
#5558 = AXIS2_PLACEMENT_3D ( 'NONE', #2181, #8286, #14398 ) ;
#5560 = B_SPLINE_CURVE_WITH_KNOTS ( 'NONE', 3,
 ( #11836, #16544, #4234, #8839, #14939, #5819 ),
 .UNSPECIFIED., .F., .F.,
 ( 4, 2, 4 ),
 ( 2.132675795045741476E-07, 0.001878604073277002386, 0.003756994878974500435 ),
 .UNSPECIFIED. ) ;
#5561 = FACE_OUTER_BOUND ( 'NONE', #14868, .T. ) ;
#5562 = EDGE_LOOP ( 'NONE', ( #14536, #9873 ) ) ;
#5563 = CARTESIAN_POINT ( 'NONE',  ( 0.5109457054261454800, -4.861323657744410554, -14.84374999795161543 ) ) ;
#5564 = DIRECTION ( 'NONE',  ( 0.000000000000000000, 0.000000000000000000, 1.000000000000000000 ) ) ;
#5565 = AXIS2_PLACEMENT_3D ( 'NONE', #3241, #6330, #17250 ) ;
#5566 = VERTEX_POINT ( 'NONE', #13130 ) ;
#5567 = CARTESIAN_POINT ( 'NONE',  ( 2.783069004973548033, 23.92277630352795370, 5.408431875071527450 ) ) ;
#5568 = VECTOR ( 'NONE', #9305, 1000.000000000000000 ) ;
#5569 = CARTESIAN_POINT ( 'NONE',  ( 0.000000000000000000, 22.25075486061737351, 9.324097380959511128 ) ) ;
#5570 = CARTESIAN_POINT ( 'NONE',  ( -4.762499999999999289, 5.832380380939268136E-16, 0.000000000000000000 ) ) ;
#5571 = CARTESIAN_POINT ( 'NONE',  ( 1.749999999999998002, 0.000000000000000000, 0.000000000000000000 ) ) ;
#5572 = DIRECTION ( 'NONE',  ( 0.000000000000000000, 0.000000000000000000, 1.000000000000000000 ) ) ;
#5573 = FACE_OUTER_BOUND ( 'NONE', #16038, .T. ) ;
#5574 = EDGE_LOOP ( 'NONE', ( #10929, #3293, #14898, #3721 ) ) ;
#5575 = CARTESIAN_POINT ( 'NONE',  ( 16.96448111170888851, 1.130229351527639370, 35.00000000000000000 ) ) ;
#5576 = DIRECTION ( 'NONE',  ( 0.000000000000000000, 0.000000000000000000, 1.000000000000000000 ) ) ;
#5577 = B_SPLINE_CURVE_WITH_KNOTS ( 'NONE', 3,
 ( #8615, #2316, #14537, #4112 ),
 .UNSPECIFIED., .F., .F.,
 ( 4, 4 ),
 ( 2.034713381942770033E-07, 0.0006887909409525396235 ),
 .UNSPECIFIED. ) ;
#5578 = UNCERTAINTY_MEASURE_WITH_UNIT (LENGTH_MEASURE( 1.000000000000000082E-05 ), #6065, 'distance_accuracy_value', 'NONE');
#5579 = CYLINDRICAL_SURFACE ( 'NONE', #3202, 3.000000000000000000 ) ;
#5580 = DIRECTION ( 'NONE',  ( 0.000000000000000000, -0.4999999999999978906, -0.8660254037844399289 ) ) ;
#5581 = DIRECTION ( 'NONE',  ( -1.000000000000000000, 0.000000000000000000, 0.000000000000000000 ) ) ;
#5582 = EDGE_CURVE ( 'NONE', #6183, #10033, #14994, .T. ) ;
#5583 = ORIENTED_EDGE ( 'NONE', *, *, #18026, .T. ) ;
#5584 = LINE ( 'NONE', #15098, #9323 ) ;
#5585 = DIRECTION ( 'NONE',  ( 0.000000000000000000, 2.061057595219972332E-15, -1.000000000000000000 ) ) ;
#5586 = ORIENTED_EDGE ( 'NONE', *, *, #14020, .T. ) ;
#5587 = CARTESIAN_POINT ( 'NONE',  ( 14.34374999795161365, -4.780397808154265960, 1.280903732194421663 ) ) ;
#5588 = DIRECTION ( 'NONE',  ( 0.000000000000000000, 0.000000000000000000, 1.000000000000000000 ) ) ;
#5589 = AXIS2_PLACEMENT_3D ( 'NONE', #3752, #9875, #5345 ) ;
#5590 = DIRECTION ( 'NONE',  ( -1.000000000000000000, -0.000000000000000000, -0.000000000000000000 ) ) ;
#5591 = DIRECTION ( 'NONE',  ( 0.000000000000000000, 0.000000000000000000, -1.000000000000000000 ) ) ;
#5592 = ORIENTED_EDGE ( 'NONE', *, *, #11944, .F. ) ;
#5593 = DIRECTION ( 'NONE',  ( 0.000000000000000000, 0.000000000000000000, -1.000000000000000000 ) ) ;
#5594 =( NAMED_UNIT ( * ) SI_UNIT ( $, .STERADIAN. ) SOLID_ANGLE_UNIT ( ) );
#5595 = DIRECTION ( 'NONE',  ( -1.000000000000000000, -0.000000000000000000, -0.000000000000000000 ) ) ;
#5596 = EDGE_CURVE ( 'NONE', #17754, #1977, #12670, .T. ) ;
#5597 = CARTESIAN_POINT ( 'NONE',  ( 11.00000000000000711, -5.700000000000001066, -3.945386292505473391E-14 ) ) ;
#5598 = EDGE_LOOP ( 'NONE', ( #16045, #15744, #2442, #18269 ) ) ;
#5599 = DIRECTION ( 'NONE',  ( -0.000000000000000000, -0.000000000000000000, 1.000000000000000000 ) ) ;
#5600 = ORIENTED_EDGE ( 'NONE', *, *, #9678, .F. ) ;
#5601 = DIRECTION ( 'NONE',  ( -1.000000000000000000, 0.000000000000000000, -0.000000000000000000 ) ) ;
#5602 = DIRECTION ( 'NONE',  ( -0.9238795325112865164, 0.3826834323650905034, 0.000000000000000000 ) ) ;
#5603 = DIRECTION ( 'NONE',  ( 0.000000000000000000, 0.000000000000000000, -1.000000000000000000 ) ) ;
#5604 = TOROIDAL_SURFACE ( 'NONE', #1775, 24.12539914357697768, 8.000000000000000000 ) ;
#5605 = CARTESIAN_POINT ( 'NONE',  ( 1.899999999999999245, 6.760799999999997034, 0.000000000000000000 ) ) ;
#5606 = EDGE_CURVE ( 'NONE', #10821, #5291, #12023, .T. ) ;
#5607 = AXIS2_PLACEMENT_3D ( 'NONE', #8131, #3629, #3730 ) ;
#5608 = ORIENTED_EDGE ( 'NONE', *, *, #4458, .T. ) ;
#5609 = CARTESIAN_POINT ( 'NONE',  ( -2.695436003842760275, -4.150607464521772094, -9.968749997951617203 ) ) ;
#5610 = CARTESIAN_POINT ( 'NONE',  ( 11.81249999590322552, -2.068159791354220900, 5.387740456496221242 ) ) ;
#5611 = ORIENTED_EDGE ( 'NONE', *, *, #15175, .F. ) ;
#5612 = CARTESIAN_POINT ( 'NONE',  ( -11.00000000000000355, -4.898587196589412829E-16, 0.000000000000000000 ) ) ;
#5613 = CARTESIAN_POINT ( 'NONE',  ( 0.02436607992776368414, 18.55949924794916228, -16.37294372382838148 ) ) ;
#5614 = ORIENTED_EDGE ( 'NONE', *, *, #3655, .F. ) ;
#5615 = AXIS2_PLACEMENT_3D ( 'NONE', #11422, #8215, #6798 ) ;
#5616 = CARTESIAN_POINT ( 'NONE',  ( 4.235925505221166176, 3.814044456245473835, -7.000000000000005329 ) ) ;
#5617 = CARTESIAN_POINT ( 'NONE',  ( 4.888101187499994893, -0.7741991708319229115, -6.968749997951614539 ) ) ;
#5618 = CARTESIAN_POINT ( 'NONE',  ( 13.00000000000000178, -3.789407127742538517, 3.087705756618167374 ) ) ;
#5619 = AXIS2_PLACEMENT_3D ( 'NONE', #4414, #19718, #15327 ) ;
#5620 = ORIENTED_EDGE ( 'NONE', *, *, #11910, .T. ) ;
#5621 = ADVANCED_FACE ( 'NONE', ( #3826 ), #19683, .T. ) ;
#5622 = CARTESIAN_POINT ( 'NONE',  ( 2.765633920072235519, 24.15498966839970052, -5.391175441198366336 ) ) ;
#5623 = ORIENTED_EDGE ( 'NONE', *, *, #2362, .F. ) ;
#5624 = DIRECTION ( 'NONE',  ( 1.000000000000000000, 0.000000000000000000, 0.000000000000000000 ) ) ;
#5625 = ORIENTED_EDGE ( 'NONE', *, *, #14312, .F. ) ;
#5626 = DIRECTION ( 'NONE',  ( -1.000000000000000000, -0.000000000000000000, -0.000000000000000000 ) ) ;
#5627 = CYLINDRICAL_SURFACE ( 'NONE', #6670, 2.524999999999996358 ) ;
#5628 = DIRECTION ( 'NONE',  ( 0.000000000000000000, 0.000000000000000000, 1.000000000000000000 ) ) ;
#5629 = VERTEX_POINT ( 'NONE', #11625 ) ;
#5630 = CARTESIAN_POINT ( 'NONE',  ( -1.510506337161893642, -4.648860486681943627, -12.46874999795161543 ) ) ;
#5631 = DIRECTION ( 'NONE',  ( 0.000000000000000000, 0.000000000000000000, 1.000000000000000000 ) ) ;
#5632 = EDGE_CURVE ( 'NONE', #4257, #13799, #6566, .T. ) ;
#5633 = DIRECTION ( 'NONE',  ( 0.000000000000000000, 0.000000000000000000, 1.000000000000000000 ) ) ;
#5634 = EDGE_LOOP ( 'NONE', ( #4284, #18522, #1417, #11359 ) ) ;
#5635 =( BOUNDED_SURFACE ( )  B_SPLINE_SURFACE ( 1, 2, ( 
 ( #10791, #13893, #186, #6269, #12396, #18487, #16091, #18782, #12687, #6660, #17486, #2371, #8178, #1974, #5370, #14184, #3869 ),
 ( #12986, #6858, #15984, #2274, #2174, #11386, #12886, #18982, #8381, #17189, #9797, #9991, #485, #3573, #9589, #8485, #14496 ) ),
 .UNSPECIFIED., .F., .F., .F. ) 
 B_SPLINE_SURFACE_WITH_KNOTS ( ( 2, 2 ),
 ( 3, 2, 2, 2, 2, 2, 2, 2, 3 ),
 ( 0.000000000000000000, 1.000000000000000000 ),
 ( 0.000000000000000000, 0.05000000000000000278, 0.1000000000000000056, 0.1499999999999999944, 0.2000000000000000111, 0.2500000000000000000, 0.2999999999999999889, 0.3499999999999999778, 0.4000000000000000222 ),
 .UNSPECIFIED. ) 
 GEOMETRIC_REPRESENTATION_ITEM ( )  RATIONAL_B_SPLINE_SURFACE ( (
 ( 1.000000000000000000, 0.9876883405951377704, 1.000000000000000000, 0.9876883405951377704, 1.000000000000000000, 0.9876883405951377704, 1.000000000000000000, 0.9876883405951377704, 1.000000000000000000, 0.9876883405951377704, 1.000000000000000000, 0.9876883405951377704, 1.000000000000000000, 0.9876883405951377704, 1.000000000000000000, 0.9876883405951377704, 1.000000000000000000),
 ( 1.000000000000000000, 0.9876883405951377704, 1.000000000000000000, 0.9876883405951377704, 1.000000000000000000, 0.9876883405951377704, 1.000000000000000000, 0.9876883405951377704, 1.000000000000000000, 0.9876883405951377704, 1.000000000000000000, 0.9876883405951377704, 1.000000000000000000, 0.9876883405951377704, 1.000000000000000000, 0.9876883405951377704, 1.000000000000000000) ) ) 
 REPRESENTATION_ITEM ( '' )  SURFACE ( )  );
#5636 = EDGE_CURVE ( 'NONE', #17537, #1730, #536, .T. ) ;
#5637 = CIRCLE ( 'NONE', #16838, 28.06981291497571362 ) ;
#5638 = CIRCLE ( 'NONE', #2133, 0.2000000000000005107 ) ;
#5639 = CARTESIAN_POINT ( 'NONE',  ( 4.476417968967386862, 17.43449690031536292, 35.00000000000000000 ) ) ;
#5640 = B_SPLINE_CURVE_WITH_KNOTS ( 'NONE', 3,
 ( #13755, #6597, #16862, #621 ),
 .UNSPECIFIED., .F., .F.,
 ( 4, 4 ),
 ( 2.135345996175604595E-07, 0.0006888010880210905865 ),
 .UNSPECIFIED. ) ;
#5641 = ORIENTED_EDGE ( 'NONE', *, *, #16786, .F. ) ;
#5642 = DIRECTION ( 'NONE',  ( 0.000000000000000000, 0.000000000000000000, 1.000000000000000000 ) ) ;
#5643 = EDGE_CURVE ( 'NONE', #11476, #2678, #17633, .T. ) ;
#5644 = CARTESIAN_POINT ( 'NONE',  ( 2.789999999999999147, -15.04425356660774682, 20.70663861606266209 ) ) ;
#5645 = DIRECTION ( 'NONE',  ( -1.000000000000000000, -0.000000000000000000, -0.000000000000000000 ) ) ;
#5646 = VERTEX_POINT ( 'NONE', #7197 ) ;
#5647 = CARTESIAN_POINT ( 'NONE',  ( 0.000000000000000000, -18.28042085475288303, 15.74360496233377305 ) ) ;
#5648 = VECTOR ( 'NONE', #11175, 1000.000000000000227 ) ;
#5649 = EDGE_CURVE ( 'NONE', #12547, #14379, #17774, .T. ) ;
#5650 = CARTESIAN_POINT ( 'NONE',  ( 5.387740456496232788, 2.068159791354184041, -11.50000000000000355 ) ) ;
#5651 = AXIS2_PLACEMENT_3D ( 'NONE', #7919, #1732, #6313 ) ;
#5652 = ORIENTED_EDGE ( 'NONE', *, *, #7278, .F. ) ;
#5653 = EDGE_LOOP ( 'NONE', ( #4620, #5850, #1556, #11471, #3454 ) ) ;
#5654 = CARTESIAN_POINT ( 'NONE',  ( -3.476417968967383754, 17.43449690031536292, -32.00000000000000000 ) ) ;
#5655 = CARTESIAN_POINT ( 'NONE',  ( 8.468749997951615427, 1.988169868018562436, 4.465502636338039011 ) ) ;
#5656 = VERTEX_POINT ( 'NONE', #10819 ) ;
#5657 = EDGE_CURVE ( 'NONE', #7394, #3602, #17136, .T. ) ;
#5658 = CARTESIAN_POINT ( 'NONE',  ( -4.888101187500000222, 0.000000000000000000, -6.468749997951615427 ) ) ;
#5659 = EDGE_LOOP ( 'NONE', ( #8614, #5583, #1587, #9564 ) ) ;
#5660 = FACE_OUTER_BOUND ( 'NONE', #11420, .T. ) ;
#5661 = CARTESIAN_POINT ( 'NONE',  ( 9.812499995903225525, -1.493657965219446160, -5.574407415329178939 ) ) ;
#5662 = CIRCLE ( 'NONE', #5353, 5.700000000000001954 ) ;
#5663 = EDGE_LOOP ( 'NONE', ( #15210, #15689, #11315, #17278, #18478, #14582, #11414, #10463 ) ) ;
#5664 = FACE_OUTER_BOUND ( 'NONE', #561, .T. ) ;
#5665 = AXIS2_PLACEMENT_3D ( 'NONE', #14305, #5749, #2551 ) ;
#5666 = EDGE_CURVE ( 'NONE', #10545, #17625, #2737, .T. ) ;
#5667 = CARTESIAN_POINT ( 'NONE',  ( 6.234374998975811266, -4.584782303107560963, -2.647025296875054057 ) ) ;
#5668 = CARTESIAN_POINT ( 'NONE',  ( 11.34374999795161543, 4.888101187500000222, -0.7741991708318890497 ) ) ;
#5669 = CARTESIAN_POINT ( 'NONE',  ( 1.749999999999998002, 0.000000000000000000, 0.000000000000000000 ) ) ;
#5670 = CARTESIAN_POINT ( 'NONE',  ( 2.790000000000077307, 20.65026423218591844, -12.51972477286559027 ) ) ;
#5671 = CARTESIAN_POINT ( 'NONE',  ( 7.937500000000000000, -0.7744039358429353204, 6.268043809681820044E-17 ) ) ;
#5672 = VERTEX_POINT ( 'NONE', #8921 ) ;
#5673 = CARTESIAN_POINT ( 'NONE',  ( 2.789999999999999147, 0.000000000000000000, 0.000000000000000000 ) ) ;
#5674 = CIRCLE ( 'NONE', #8246, 3.000000000000000000 ) ;
#5675 = LINE ( 'NONE', #3791, #8417 ) ;
#5676 = CARTESIAN_POINT ( 'NONE',  ( -36.00000000000000000, -5.000000000000000888, 2.000000000000000000 ) ) ;
#5677 = AXIS2_PLACEMENT_3D ( 'NONE', #5605, #2321, #5703 ) ;
#5678 = CARTESIAN_POINT ( 'NONE',  ( -3.968750000000000000, 4.860316984116057109E-16, -6.527800000000000047 ) ) ;
#5679 = CARTESIAN_POINT ( 'NONE',  ( -16.96448111170888851, 1.130229351527647585, 32.00000000000000000 ) ) ;
#5680 = ORIENTED_EDGE ( 'NONE', *, *, #662, .T. ) ;
#5681 = DIRECTION ( 'NONE',  ( -1.000000000000000000, -0.000000000000000000, -0.000000000000000000 ) ) ;
#5682 = CARTESIAN_POINT ( 'NONE',  ( 10.12500000000000178, 4.898587196589412829E-16, -4.000000000000000000 ) ) ;
#5683 = ORIENTED_EDGE ( 'NONE', *, *, #13076, .F. ) ;
#5684 = FACE_OUTER_BOUND ( 'NONE', #19612, .T. ) ;
#5685 = ADVANCED_FACE ( 'NONE', ( #7703 ), #4616, .F. ) ;
#5686 = DIRECTION ( 'NONE',  ( 1.000000000000000000, 0.000000000000000000, 0.000000000000000000 ) ) ;
#5687 = AXIS2_PLACEMENT_3D ( 'NONE', #11381, #7042, #12071 ) ;
#5688 = CARTESIAN_POINT ( 'NONE',  ( 1.039999999999995817, 27.76164181293051669, 4.147968289691385202 ) ) ;
#5689 = CARTESIAN_POINT ( 'NONE',  ( 2.789999999999999147, 24.44424927289185945, 12.96989951879416125 ) ) ;
#5690 = EDGE_LOOP ( 'NONE', ( #13793, #9145, #16402, #11237 ) ) ;
#5691 = CARTESIAN_POINT ( 'NONE',  ( 8.968749997951611874, 3.499494075959816541, -3.499494075959816541 ) ) ;
#5692 = DIRECTION ( 'NONE',  ( 0.000000000000000000, 0.000000000000000000, 1.000000000000000000 ) ) ;
#5693 = ADVANCED_FACE ( 'NONE', ( #7807 ), #16623, .T. ) ;
#5694 = CARTESIAN_POINT ( 'NONE',  ( 9.000000000000005329, -4.611396867937225252, 3.350375938067065462 ) ) ;
#5695 = EDGE_LOOP ( 'NONE', ( #7643, #9033 ) ) ;
#5696 = CARTESIAN_POINT ( 'NONE',  ( -2.500000000000000888, 8.073750000000021743, 0.000000000000000000 ) ) ;
#5697 = ORIENTED_EDGE ( 'NONE', *, *, #10847, .F. ) ;
#5698 = FACE_OUTER_BOUND ( 'NONE', #9534, .T. ) ;
#5699 = LINE ( 'NONE', #13313, #13011 ) ;
#5700 = CARTESIAN_POINT ( 'NONE',  ( -3.954556930911881096, -2.873153789725797935, -14.84374999795161543 ) ) ;
#5701 = TOROIDAL_SURFACE ( 'NONE', #15633, 24.12539914357697413, 8.000000000000000000 ) ;
#5702 = ADVANCED_FACE ( 'NONE', ( #15229 ), #11701, .T. ) ;
#5703 = DIRECTION ( 'NONE',  ( -0.000000000000000000, 0.000000000000000000, -1.000000000000000000 ) ) ;
#5704 = ORIENTED_EDGE ( 'NONE', *, *, #13766, .F. ) ;
#5705 = DIRECTION ( 'NONE',  ( 0.000000000000000000, 0.000000000000000000, -1.000000000000000000 ) ) ;
#5706 = DIRECTION ( 'NONE',  ( 0.000000000000000000, 0.000000000000000000, 1.000000000000000000 ) ) ;
#5707 = ORIENTED_EDGE ( 'NONE', *, *, #8237, .T. ) ;
#5708 = PLANE ( 'NONE',  #16037 ) ;
#5709 = CARTESIAN_POINT ( 'NONE',  ( -1.761396867937238042, -5.421022142882365280, -13.31249999590322730 ) ) ;
#5710 = VECTOR ( 'NONE', #1864, 1000.000000000000000 ) ;
#5711 = VERTEX_POINT ( 'NONE', #7604 ) ;
#5712 = APPLICATION_CONTEXT ( 'automotive_design' ) ;
#5713 = CARTESIAN_POINT ( 'NONE',  ( 1.280903732194454303, 4.780397808154257078, -9.343749997951615427 ) ) ;
#5714 = LINE ( 'NONE', #14934, #12979 ) ;
#5715 = CARTESIAN_POINT ( 'NONE',  ( 1.869200000000000195, 0.000000000000000000, 0.000000000000000000 ) ) ;
#5716 = EDGE_CURVE ( 'NONE', #14637, #9343, #19365, .T. ) ;
#5717 = EDGE_LOOP ( 'NONE', ( #14080, #17671, #6970, #2222 ) ) ;
#5718 = CARTESIAN_POINT ( 'NONE',  ( 12.00000000000000355, 0.000000000000000000, 0.000000000000000000 ) ) ;
#5719 = ORIENTED_EDGE ( 'NONE', *, *, #11368, .F. ) ;
#5720 = CYLINDRICAL_SURFACE ( 'NONE', #6915, 9.000000000000000000 ) ;
#5721 = EDGE_LOOP ( 'NONE', ( #13208, #11260 ) ) ;
#5722 = CIRCLE ( 'NONE', #1906, 0.1999999999999987899 ) ;
#5723 = FILL_AREA_STYLE_COLOUR ( '', #14708 ) ;
#5724 = DIRECTION ( 'NONE',  ( 0.000000000000000000, 0.000000000000000000, 1.000000000000000000 ) ) ;
#5725 = LINE ( 'NONE', #10063, #3475 ) ;
#5726 = CARTESIAN_POINT ( 'NONE',  ( 12.96874999795161543, -0.2590123213420631454, -4.942249507334558700 ) ) ;
#5727 = DIRECTION ( 'NONE',  ( 1.000000000000000000, 0.000000000000000000, 0.000000000000000000 ) ) ;
#5728 = ORIENTED_EDGE ( 'NONE', *, *, #5135, .F. ) ;
#5729 = CARTESIAN_POINT ( 'NONE',  ( 12.00000000000000355, 4.898587196589412829E-16, 4.000000000000000000 ) ) ;
#5730 = EDGE_CURVE ( 'NONE', #7686, #18594, #14138, .T. ) ;
#5731 = EDGE_CURVE ( 'NONE', #8313, #8718, #16530, .T. ) ;
#5732 = AXIS2_PLACEMENT_3D ( 'NONE', #17332, #18829, #10934 ) ;
#5733 = EDGE_LOOP ( 'NONE', ( #14036, #14403, #7433, #12296 ) ) ;
#5734 = CIRCLE ( 'NONE', #8308, 1.000000000000004441 ) ;
#5735 = DIRECTION ( 'NONE',  ( 1.000000000000000000, 0.000000000000000000, 0.000000000000000000 ) ) ;
#5736 = EDGE_CURVE ( 'NONE', #479, #15528, #4985, .T. ) ;
#5737 = DIRECTION ( 'NONE',  ( 1.000000000000000000, 0.000000000000000000, 0.000000000000000000 ) ) ;
#5738 = DIRECTION ( 'NONE',  ( 1.000000000000000000, 0.000000000000000000, 0.000000000000000000 ) ) ;
#5739 = DIRECTION ( 'NONE',  ( 6.419766481290786633E-33, -1.000000000000000000, 0.000000000000000000 ) ) ;
#5740 = VERTEX_POINT ( 'NONE', #7501 ) ;
#5741 = DIRECTION ( 'NONE',  ( 0.000000000000000000, 0.000000000000000000, 1.000000000000000000 ) ) ;
#5742 = EDGE_LOOP ( 'NONE', ( #16268, #6360 ) ) ;
#5743 = CARTESIAN_POINT ( 'NONE',  ( -2.849999999999988987, 4.936344801571308061, -6.000000000000005329 ) ) ;
#5744 = DIRECTION ( 'NONE',  ( 1.000000000000000000, 0.000000000000000000, 0.000000000000000000 ) ) ;
#5745 = VERTEX_POINT ( 'NONE', #10622 ) ;
#5746 = ORIENTED_EDGE ( 'NONE', *, *, #378, .T. ) ;
#5747 = DIRECTION ( 'NONE',  ( 0.000000000000000000, 0.000000000000000000, 1.000000000000000000 ) ) ;
#5748 = VECTOR ( 'NONE', #15490, 1000.000000000000000 ) ;
#5749 = DIRECTION ( 'NONE',  ( 1.000000000000000000, 0.000000000000000000, 0.000000000000000000 ) ) ;
#5750 = CIRCLE ( 'NONE', #11210, 4.824999999999999289 ) ;
#5751 = ORIENTED_EDGE ( 'NONE', *, *, #3212, .F. ) ;
#5752 = CARTESIAN_POINT ( 'NONE',  ( 5.700000000000001066, 0.5990941410143489909, -12.33180101230371584 ) ) ;
#5753 = VERTEX_POINT ( 'NONE', #9319 ) ;
#5754 = CARTESIAN_POINT ( 'NONE',  ( -2.850000000000058265, -4.936344801571268093, -7.312499995903225525 ) ) ;
#5755 = DIRECTION ( 'NONE',  ( -1.000000000000000000, -0.000000000000000000, 0.000000000000000000 ) ) ;
#5756 = VERTEX_POINT ( 'NONE', #214 ) ;
#5757 = CARTESIAN_POINT ( 'NONE',  ( 3.968750000000000000, 0.000000000000000000, -6.527800000000000047 ) ) ;
#5758 = AXIS2_PLACEMENT_3D ( 'NONE', #15155, #15056, #1348 ) ;
#5759 = AXIS2_PLACEMENT_3D ( 'NONE', #15270, #6144, #12263 ) ;
#5760 = ADVANCED_FACE ( 'NONE', ( #15422 ), #18726, .T. ) ;
#5761 = CARTESIAN_POINT ( 'NONE',  ( -4.465502636338010589, 1.988169868018623720, -14.84374999795161543 ) ) ;
#5762 = CARTESIAN_POINT ( 'NONE',  ( -3.968750000000004441, 6.874076642538978987, 0.000000000000000000 ) ) ;
#5763 = CARTESIAN_POINT ( 'NONE',  ( 12.92161831991541554, 0.8983569717629179552, 4.806352606718987452 ) ) ;
#5764 = EDGE_CURVE ( 'NONE', #11950, #8225, #13720, .T. ) ;
#5765 = CARTESIAN_POINT ( 'NONE',  ( -10.00000000000000000, 0.000000000000000000, 0.000000000000000000 ) ) ;
#5766 = PLANE ( 'NONE',  #15726 ) ;
#5767 = ORIENTED_EDGE ( 'NONE', *, *, #5430, .T. ) ;
#5768 = CARTESIAN_POINT ( 'NONE',  ( 1.749999999999998002, 27.68468304288259318, 4.633866840649019103 ) ) ;
#5769 = FACE_BOUND ( 'NONE', #19427, .T. ) ;
#5770 = UNCERTAINTY_MEASURE_WITH_UNIT (LENGTH_MEASURE( 1.000000000000000082E-05 ), #675, 'distance_accuracy_value', 'NONE');
#5771 = CARTESIAN_POINT ( 'NONE',  ( 4.611396867937201272, 3.350375938067098325, 0.000000000000000000 ) ) ;
#5772 = EDGE_CURVE ( 'NONE', #19129, #9230, #9019, .T. ) ;
#5773 = CARTESIAN_POINT ( 'NONE',  ( 2.000000000000001776, 9.887492094615969966E-16, 8.073750000000021743 ) ) ;
#5774 = AXIS2_PLACEMENT_3D ( 'NONE', #13650, #7530, #7832 ) ;
#5775 = ORIENTED_EDGE ( 'NONE', *, *, #8109, .F. ) ;
#5776 = CARTESIAN_POINT ( 'NONE',  ( -34.92499999999994742, 0.000000000000000000, 0.000000000000000000 ) ) ;
#5777 = CIRCLE ( 'NONE', #3557, 1.000000000000000888 ) ;
#5778 = DIRECTION ( 'NONE',  ( -1.000000000000000000, 0.000000000000000000, 0.000000000000000000 ) ) ;
#5779 = ORIENTED_EDGE ( 'NONE', *, *, #18937, .F. ) ;
#5780 = CARTESIAN_POINT ( 'NONE',  ( 9.843749997951615427, 0.5109457054261445919, 4.861323657744411442 ) ) ;
#5781 = EDGE_CURVE ( 'NONE', #2115, #13534, #4677, .T. ) ;
#5782 = CARTESIAN_POINT ( 'NONE',  ( 8.812499995903225525, -5.763142191869158992, 0.3020334839682081163 ) ) ;
#5783 = CARTESIAN_POINT ( 'NONE',  ( 11.96874999795161365, 3.114526743279308896, -3.846120219227901149 ) ) ;
#5784 = CARTESIAN_POINT ( 'NONE',  ( 2.789999999999999147, 9.324097380959445402, 22.25075486061742325 ) ) ;
#5785 = EDGE_LOOP ( 'NONE', ( #18529, #17223 ) ) ;
#5786 = AXIS2_PLACEMENT_3D ( 'NONE', #8725, #8443, #17639 ) ;
#5787 = AXIS2_PLACEMENT_3D ( 'NONE', #19595, #8598, #1194 ) ;
#5788 = CARTESIAN_POINT ( 'NONE',  ( 8.000000000000000000, 9.797174393178825657E-16, -29.00000000000000000 ) ) ;
#5789 = DIRECTION ( 'NONE',  ( 1.000000000000000000, 0.000000000000000000, 0.000000000000000000 ) ) ;
#5790 = DIRECTION ( 'NONE',  ( 1.000000000000000000, 0.000000000000000000, 0.000000000000000000 ) ) ;
#5791 = ORIENTED_EDGE ( 'NONE', *, *, #1143, .F. ) ;
#5792 = CARTESIAN_POINT ( 'NONE',  ( 0.02436607992776064838, 12.59161484032912171, 21.30679549418635688 ) ) ;
#5793 = ORIENTED_EDGE ( 'NONE', *, *, #6862, .F. ) ;
#5794 = B_SPLINE_CURVE_WITH_KNOTS ( 'NONE', 3,
 ( #18248, #4437, #2827, #6024 ),
 .UNSPECIFIED., .F., .F.,
 ( 4, 4 ),
 ( 0.000000000000000000, 0.001125480700308659687 ),
 .UNSPECIFIED. ) ;
#5795 = CARTESIAN_POINT ( 'NONE',  ( -1.000000000000001998, 18.00000000000000355, -32.00000000000000000 ) ) ;
#5796 = CARTESIAN_POINT ( 'NONE',  ( 8.843749997951615427, 2.873153789725825469, -3.954556930911862000 ) ) ;
#5797 = EDGE_CURVE ( 'NONE', #2850, #7268, #17930, .T. ) ;
#5798 = CARTESIAN_POINT ( 'NONE',  ( 13.00000000000000000, -4.333424887442987483, -2.261628166637620119 ) ) ;
#5799 = B_SPLINE_CURVE_WITH_KNOTS ( 'NONE', 1,
 ( #8353, #3650 ),
 .UNSPECIFIED., .F., .F.,
 ( 2, 2 ),
 ( 0.000000000000000000, 1.000000000000000000 ),
 .UNSPECIFIED. ) ;
#5800 = LINE ( 'NONE', #16526, #10805 ) ;
#5801 = EDGE_LOOP ( 'NONE', ( #1409, #1564, #7140, #11046 ) ) ;
#5802 = CARTESIAN_POINT ( 'NONE',  ( 2.000000000000001776, 0.000000000000000000, 0.000000000000000000 ) ) ;
#5803 = DIRECTION ( 'NONE',  ( 0.000000000000000000, 0.000000000000000000, 1.000000000000000000 ) ) ;
#5804 = EDGE_CURVE ( 'NONE', #17520, #15780, #4663, .T. ) ;
#5805 = AXIS2_PLACEMENT_3D ( 'NONE', #11418, #818, #9929 ) ;
#5806 = EDGE_LOOP ( 'NONE', ( #16165, #15552, #17610, #2531 ) ) ;
#5807 = AXIS2_PLACEMENT_3D ( 'NONE', #6762, #9897, #1268 ) ;
#5808 = CIRCLE ( 'NONE', #10941, 8.239200000000002078 ) ;
#5809 = DIRECTION ( 'NONE',  ( -1.000000000000000000, 0.000000000000000000, 0.000000000000000000 ) ) ;
#5810 = DIRECTION ( 'NONE',  ( 0.000000000000000000, 0.000000000000000000, -1.000000000000000000 ) ) ;
#5811 = ORIENTED_EDGE ( 'NONE', *, *, #17071, .F. ) ;
#5812 = CARTESIAN_POINT ( 'NONE',  ( 4.861323657744406113, -0.5109457054261780096, -13.84374999795161543 ) ) ;
#5813 = EDGE_CURVE ( 'NONE', #15303, #8962, #10113, .T. ) ;
#5814 = CARTESIAN_POINT ( 'NONE',  ( 12.31249999590322552, 2.849999999999989875, 4.936344801571308061 ) ) ;
#5815 = FACE_BOUND ( 'NONE', #8607, .T. ) ;
#5816 = ORIENTED_EDGE ( 'NONE', *, *, #8190, .T. ) ;
#5817 = DIRECTION ( 'NONE',  ( 1.000000000000000000, 0.000000000000000000, 0.000000000000000000 ) ) ;
#5818 = ORIENTED_EDGE ( 'NONE', *, *, #7312, .T. ) ;
#5819 = CARTESIAN_POINT ( 'NONE',  ( 1.039999999999995817, -27.76164181293048472, -4.147968289691575272 ) ) ;
#5820 = VECTOR ( 'NONE', #771, 1000.000000000000000 ) ;
#5821 = ORIENTED_EDGE ( 'NONE', *, *, #16872, .T. ) ;
#5822 = FACE_OUTER_BOUND ( 'NONE', #18098, .T. ) ;
#5823 = AXIS2_PLACEMENT_3D ( 'NONE', #2732, #14949, #19537 ) ;
#5824 = LINE ( 'NONE', #10642, #13454 ) ;
#5825 = ADVANCED_FACE ( 'NONE', ( #15716 ), #310, .F. ) ;
#5826 = CARTESIAN_POINT ( 'NONE',  ( -2.873153789725852558, -3.954556930911842016, -13.84374999795161543 ) ) ;
#5827 = DIRECTION ( 'NONE',  ( -0.000000000000000000, -0.000000000000000000, -1.000000000000000000 ) ) ;
#5828 = AXIS2_PLACEMENT_3D ( 'NONE', #5230, #11347, #3439 ) ;
#5829 = B_SPLINE_CURVE_WITH_KNOTS ( 'NONE', 3,
 ( #8547, #2432, #1038, #8456, #17460, #19240 ),
 .UNSPECIFIED., .F., .F.,
 ( 4, 2, 4 ),
 ( 4.462636882155291330E-07, 0.001879885203074804561, 0.003759324142461393896 ),
 .UNSPECIFIED. ) ;
#5830 = CARTESIAN_POINT ( 'NONE',  ( 12.99999999999999467, 0.4594918047638986702, 4.866883308198427294 ) ) ;
#5831 = ORIENTED_EDGE ( 'NONE', *, *, #10428, .F. ) ;
#5832 = VECTOR ( 'NONE', #3171, 1000.000000000000000 ) ;
#5833 = LINE ( 'NONE', #1339, #5468 ) ;
#5834 = ADVANCED_FACE ( 'NONE', ( #3507 ), #3413, .F. ) ;
#5835 = CARTESIAN_POINT ( 'NONE',  ( 2.030753605846573606, -3.797885586973408056, 27.31305418910209326 ) ) ;
#5836 = VERTEX_POINT ( 'NONE', #14416 ) ;
#5837 = DIRECTION ( 'NONE',  ( 1.000000000000000000, 0.000000000000000000, 0.000000000000000000 ) ) ;
#5838 = CARTESIAN_POINT ( 'NONE',  ( -3.968750000000000000, 4.860316984116057109E-16, -5.946610266546040968 ) ) ;
#5839 = LINE ( 'NONE', #4152, #1307 ) ;
#5840 = VECTOR ( 'NONE', #10947, 1000.000000000000000 ) ;
#5841 = CARTESIAN_POINT ( 'NONE',  ( 4.781284448697187273, -1.016293382781444654, -10.46874999795161720 ) ) ;
#5842 = AXIS2_PLACEMENT_3D ( 'NONE', #14513, #14605, #19094 ) ;
#5843 = FACE_BOUND ( 'NONE', #4711, .T. ) ;
#5844 = VERTEX_POINT ( 'NONE', #1905 ) ;
#5845 = CARTESIAN_POINT ( 'NONE',  ( 2.789999999999999591, 2.133490293297010343, 24.22479935914660132 ) ) ;
#5846 = CARTESIAN_POINT ( 'NONE',  ( -4.233219804643904460, -2.444050593749961031, -11.46874999795161543 ) ) ;
#5847 =( LENGTH_UNIT ( ) NAMED_UNIT ( * ) SI_UNIT ( .MILLI., .METRE. ) );
#5848 = ORIENTED_EDGE ( 'NONE', *, *, #17371, .T. ) ;
#5849 = ADVANCED_FACE ( 'NONE', ( #12620 ), #6390, .T. ) ;
#5850 = ORIENTED_EDGE ( 'NONE', *, *, #1908, .T. ) ;
#5851 = CARTESIAN_POINT ( 'NONE',  ( -2.500000000000002220, 1.089935651241146723E-15, 8.800000000000022027 ) ) ;
#5852 = MECHANICAL_DESIGN_GEOMETRIC_PRESENTATION_REPRESENTATION (  '', ( #3306 ), #9734 ) ;
#5853 = CARTESIAN_POINT ( 'NONE',  ( 8.968749997951611874, 1.280903732194421218, 4.780397808154266848 ) ) ;
#5854 = VERTEX_POINT ( 'NONE', #6296 ) ;
#5855 = CARTESIAN_POINT ( 'NONE',  ( -5.021782490506605967, 2.235841616153737998, -14.11718749948790830 ) ) ;
#5856 = VERTEX_POINT ( 'NONE', #6688 ) ;
#5857 = EDGE_CURVE ( 'NONE', #4951, #6213, #4348, .T. ) ;
#5858 = DIRECTION ( 'NONE',  ( 0.000000000000000000, 0.000000000000000000, -1.000000000000000000 ) ) ;
#5859 = CIRCLE ( 'NONE', #5225, 6.799999999999998046 ) ;
#5860 = CYLINDRICAL_SURFACE ( 'NONE', #12839, 1.000000000000000888 ) ;
#5861 = VERTEX_POINT ( 'NONE', #12716 ) ;
#5862 = B_SPLINE_CURVE_WITH_KNOTS ( 'NONE', 3,
 ( #7080, #2493, #17425, #4007 ),
 .UNSPECIFIED., .F., .F.,
 ( 4, 4 ),
 ( 3.059063720746937335E-07, 0.0006888942284914101538 ),
 .UNSPECIFIED. ) ;
#5863 = B_SPLINE_CURVE_WITH_KNOTS ( 'NONE', 3,
 ( #15757, #8144, #15461, #7840 ),
 .UNSPECIFIED., .F., .F.,
 ( 4, 4 ),
 ( 0.000000000000000000, 0.001125480700308659687 ),
 .UNSPECIFIED. ) ;
#5864 = CARTESIAN_POINT ( 'NONE',  ( -1.800000000000000044, 0.000000000000000000, 0.000000000000000000 ) ) ;
#5865 = CARTESIAN_POINT ( 'NONE',  ( 2.500000000000002220, 0.000000000000000000, 0.000000000000000000 ) ) ;
#5866 = LINE ( 'NONE', #9180, #11037 ) ;
#5867 = PRODUCT_DEFINITION_SHAPE ( 'NONE', 'NONE',  #19794 ) ;
#5868 = ORIENTED_EDGE ( 'NONE', *, *, #1760, .T. ) ;
#5869 = DIRECTION ( 'NONE',  ( 1.000000000000000000, 0.000000000000000000, 0.000000000000000000 ) ) ;
#5870 = DIRECTION ( 'NONE',  ( 0.000000000000000000, 0.000000000000000000, -1.000000000000000000 ) ) ;
#5871 = AXIS2_PLACEMENT_3D ( 'NONE', #5865, #19769, #10290 ) ;
#5872 = ORIENTED_EDGE ( 'NONE', *, *, #13403, .T. ) ;
#5873 = ADVANCED_FACE ( 'NONE', ( #1810 ), #15817, .T. ) ;
#5874 = LINE ( 'NONE', #2975, #16561 ) ;
#5875 = LINE ( 'NONE', #10495, #7557 ) ;
#5876 = CARTESIAN_POINT ( 'NONE',  ( 5.626241948324195441, -16.73597674598852691, -35.00000000000000000 ) ) ;
#5877 = PLANE ( 'NONE',  #16058 ) ;
#5878 = CIRCLE ( 'NONE', #8132, 1.000000000000004441 ) ;
#5879 = DIRECTION ( 'NONE',  ( 0.000000000000000000, 0.000000000000000000, 1.000000000000000000 ) ) ;
#5880 = ORIENTED_EDGE ( 'NONE', *, *, #5386, .T. ) ;
#5881 = CARTESIAN_POINT ( 'NONE',  ( 1.039999999999996927, -25.12109765559644714, -12.52377138324250438 ) ) ;
#5882 = EDGE_CURVE ( 'NONE', #17411, #2524, #9424, .T. ) ;
#5883 = CYLINDRICAL_SURFACE ( 'NONE', #12992, 28.06981291497571362 ) ;
#5884 = ORIENTED_EDGE ( 'NONE', *, *, #17932, .F. ) ;
#5885 = DIRECTION ( 'NONE',  ( -0.000000000000000000, -0.000000000000000000, 1.000000000000000000 ) ) ;
#5886 = AXIS2_PLACEMENT_3D ( 'NONE', #15313, #7589, #13402 ) ;
#5888 = CARTESIAN_POINT ( 'NONE',  ( 2.789999999999999147, -5.535312321042889394, 23.48180575137727999 ) ) ;
#5887 = ADVANCED_BREP_SHAPE_REPRESENTATION ( '', ( #9128, #16724 ), #6818 ) ;
#5889 = CARTESIAN_POINT ( 'NONE',  ( 10.00000000000000533, 4.235925505221138643, 3.814044456245502701 ) ) ;
#5890 = EDGE_CURVE ( 'NONE', #12338, #6948, #2198, .T. ) ;
#5891 = VERTEX_POINT ( 'NONE', #5007 ) ;
#5892 = AXIS2_PLACEMENT_3D ( 'NONE', #6028, #7830, #2930 ) ;
#5893 = CYLINDRICAL_SURFACE ( 'NONE', #4052, 8.265000000000021885 ) ;
#5894 = SURFACE_STYLE_FILL_AREA ( #12206 ) ;
#5895 = LINE ( 'NONE', #18113, #10388 ) ;
#5896 = CARTESIAN_POINT ( 'NONE',  ( 9.500000000000003553, -5.142044285764769462, 2.620002426024508502 ) ) ;
#5897 = VERTEX_POINT ( 'NONE', #15521 ) ;
#5898 = DIRECTION ( 'NONE',  ( -0.000000000000000000, 0.000000000000000000, 1.000000000000000000 ) ) ;
#5899 = ORIENTED_EDGE ( 'NONE', *, *, #18807, .F. ) ;
#5900 = EDGE_CURVE ( 'NONE', #1741, #13180, #2639, .T. ) ;
#5901 = CARTESIAN_POINT ( 'NONE',  ( 10.96874999795161720, -4.888101187500005551, 0.7741991708318548548 ) ) ;
#5902 = FACE_OUTER_BOUND ( 'NONE', #17006, .T. ) ;
#5903 = DIRECTION ( 'NONE',  ( 0.000000000000000000, 0.000000000000000000, 1.000000000000000000 ) ) ;
#5904 = CARTESIAN_POINT ( 'NONE',  ( 3.270778111535338262, 3.632567103900524064, -10.84374999795161543 ) ) ;
#5905 = VERTEX_POINT ( 'NONE', #14215 ) ;
#5906 = CARTESIAN_POINT ( 'NONE',  ( -4.942249507334558700, -0.2590123213420631454, -12.96874999795161543 ) ) ;
#5907 = CARTESIAN_POINT ( 'NONE',  ( -41.99999999999999289, 1.999999999999998224, 5.000000000000000000 ) ) ;
#5908 = AXIS2_PLACEMENT_3D ( 'NONE', #10092, #6962, #2375 ) ;
#5909 = ORIENTED_EDGE ( 'NONE', *, *, #2004, .T. ) ;
#5910 = VECTOR ( 'NONE', #17937, 999.9999999999998863 ) ;
#5911 = CARTESIAN_POINT ( 'NONE',  ( -4.648860486681953397, 1.510506337161861445, -7.843749997951614539 ) ) ;
#5912 = CARTESIAN_POINT ( 'NONE',  ( 2.031033471609898555, 27.31260702007175567, -3.797536611356413516 ) ) ;
#5913 = EDGE_LOOP ( 'NONE', ( #17559, #10881, #5961, #16495, #8029, #6339, #12480, #3054, #17833, #18878 ) ) ;
#5914 = CARTESIAN_POINT ( 'NONE',  ( 2.765633920072238183, -18.55949924794904504, 16.37294372382852004 ) ) ;
#5915 = CARTESIAN_POINT ( 'NONE',  ( 9.968749997951615427, 4.409619785863906571, -2.246813503491833508 ) ) ;
#5916 = EDGE_LOOP ( 'NONE', ( #12073, #5975, #18753, #8777 ) ) ;
#5917 = CARTESIAN_POINT ( 'NONE',  ( 2.765633920072235963, -24.63872515616080960, -2.336989772644527008 ) ) ;
#5918 = ORIENTED_EDGE ( 'NONE', *, *, #14122, .T. ) ;
#5919 = DIRECTION ( 'NONE',  ( 1.000000000000000000, 6.419766481290786633E-33, -0.000000000000000000 ) ) ;
#5920 = VECTOR ( 'NONE', #6037, 1000.000000000000000 ) ;
#5921 = ORIENTED_EDGE ( 'NONE', *, *, #17482, .F. ) ;
#5922 = CARTESIAN_POINT ( 'NONE',  ( 0.1882238552569850676, 23.64332819722396195, -10.68696068830383084 ) ) ;
#5923 = CIRCLE ( 'NONE', #4021, 2.524999999999998135 ) ;
#5924 = DIRECTION ( 'NONE',  ( 1.000000000000000000, 0.000000000000000000, 0.000000000000000000 ) ) ;
#5925 = CARTESIAN_POINT ( 'NONE',  ( -1.310841663519413114, 0.000000000000000000, 0.000000000000000000 ) ) ;
#5926 = CARTESIAN_POINT ( 'NONE',  ( 6.000000000000005329, -4.936344801571327601, 2.849999999999954348 ) ) ;
#5927 = CARTESIAN_POINT ( 'NONE',  ( 2.262072706628475149, 19.66369668717060293, -18.56460150496918260 ) ) ;
#5928 = ORIENTED_EDGE ( 'NONE', *, *, #11293, .T. ) ;
#5929 = CYLINDRICAL_SURFACE ( 'NONE', #18614, 1.000000000000002887 ) ;
#5930 = CYLINDRICAL_SURFACE ( 'NONE', #14859, 4.500000000000000000 ) ;
#5931 = CIRCLE ( 'NONE', #7852, 4.000000000000000000 ) ;
#5932 = VERTEX_POINT ( 'NONE', #11014 ) ;
#5933 = CIRCLE ( 'NONE', #14585, 0.9999999999999974465 ) ;
#5934 = CARTESIAN_POINT ( 'NONE',  ( 0.1882238552569851786, -23.64332819722389090, 10.68696068830398360 ) ) ;
#5935 = DIRECTION ( 'NONE',  ( 0.000000000000000000, 0.000000000000000000, 1.000000000000000000 ) ) ;
#5936 = B_SPLINE_CURVE_WITH_KNOTS ( 'NONE', 3,
 ( #1802, #17112, #3303, #10812 ),
 .UNSPECIFIED., .F., .F.,
 ( 4, 4 ),
 ( 0.005258139959819257275, 0.005342776758202955750 ),
 .UNSPECIFIED. ) ;
#5937 = VERTEX_POINT ( 'NONE', #12813 ) ;
#5938 = DIRECTION ( 'NONE',  ( 0.8660254037844398178, 0.000000000000000000, 0.4999999999999979461 ) ) ;
#5939 = CARTESIAN_POINT ( 'NONE',  ( -90.00000000000000000, 0.000000000000000000, 0.000000000000000000 ) ) ;
#5940 = CARTESIAN_POINT ( 'NONE',  ( 0.000000000000000000, 0.000000000000000000, 0.000000000000000000 ) ) ;
#5941 = ORIENTED_EDGE ( 'NONE', *, *, #3034, .T. ) ;
#5942 = DIRECTION ( 'NONE',  ( 0.000000000000000000, 1.000000000000000000, -1.224646799147353207E-16 ) ) ;
#5943 = ORIENTED_EDGE ( 'NONE', *, *, #17482, .T. ) ;
#5944 = CARTESIAN_POINT ( 'NONE',  ( 0.000000000000000000, 0.000000000000000000, 0.000000000000000000 ) ) ;
#5945 = LINE ( 'NONE', #19454, #3281 ) ;
#5946 = EDGE_CURVE ( 'NONE', #411, #11096, #8513, .T. ) ;
#5947 = PLANE ( 'NONE',  #9584 ) ;
#5948 = ORIENTED_EDGE ( 'NONE', *, *, #7977, .F. ) ;
#5949 = EDGE_LOOP ( 'NONE', ( #17232, #381, #9889, #10604 ) ) ;
#5950 = CARTESIAN_POINT ( 'NONE',  ( 6.000000000000005329, 0.000000000000000000, 0.000000000000000000 ) ) ;
#5951 = CARTESIAN_POINT ( 'NONE',  ( -22.00000000000000355, 0.000000000000000000, -32.00000000000000000 ) ) ;
#5952 = VECTOR ( 'NONE', #7677, 1000.000000000000000 ) ;
#5953 = ORIENTED_EDGE ( 'NONE', *, *, #17613, .T. ) ;
#5954 = PLANE ( 'NONE',  #19349 ) ;
#5955 = ORIENTED_EDGE ( 'NONE', *, *, #74, .T. ) ;
#5956 = DIRECTION ( 'NONE',  ( 0.000000000000000000, 0.000000000000000000, -1.000000000000000000 ) ) ;
#5957 = VERTEX_POINT ( 'NONE', #18907 ) ;
#5958 = AXIS2_PLACEMENT_3D ( 'NONE', #9086, #16887, #6351 ) ;
#5959 = VECTOR ( 'NONE', #17209, 1000.000000000000000 ) ;
#5960 = DIRECTION ( 'NONE',  ( 0.000000000000000000, 0.000000000000000000, 1.000000000000000000 ) ) ;
#5961 = ORIENTED_EDGE ( 'NONE', *, *, #12376, .T. ) ;
#5962 = CARTESIAN_POINT ( 'NONE',  ( -1.000000000000001998, 18.00000000000000355, 32.00000000000000000 ) ) ;
#5963 = CARTESIAN_POINT ( 'NONE',  ( -1.255998204157475318, -17.85806462366060288, -35.00000000000000000 ) ) ;
#5964 = ADVANCED_FACE ( 'NONE', ( #518 ), #17419, .F. ) ;
#5965 = VERTEX_POINT ( 'NONE', #11213 ) ;
#5966 = CARTESIAN_POINT ( 'NONE',  ( 6.626241948324199882, -16.73597674598852691, 35.00000000000000000 ) ) ;
#5967 = DIRECTION ( 'NONE',  ( 1.000000000000000000, 0.000000000000000000, 0.000000000000000000 ) ) ;
#5968 = PRODUCT_DEFINITION_CONTEXT ( 'detailed design', #16983, 'design' ) ;
#5969 = CARTESIAN_POINT ( 'NONE',  ( -41.99999999999999289, -4.400000000000004796, 5.388445916248358943E-16 ) ) ;
#5970 = B_SPLINE_CURVE_WITH_KNOTS ( 'NONE', 3,
 ( #1850, #7941, #3150, #15366, #14051, #7748 ),
 .UNSPECIFIED., .F., .F.,
 ( 4, 2, 4 ),
 ( 2.032124546189621919E-07, 0.001878594002992312268, 0.003756984793530005265 ),
 .UNSPECIFIED. ) ;
#5971 = CARTESIAN_POINT ( 'NONE',  ( 2.789999999999999147, -9.836394144775869819, 22.71065055754449347 ) ) ;
#5972 = VECTOR ( 'NONE', #10034, 1000.000000000000000 ) ;
#5973 = CARTESIAN_POINT ( 'NONE',  ( 13.00000000000000000, 4.362347728716210682, 2.206210144330583933 ) ) ;
#5974 = CIRCLE ( 'NONE', #5033, 0.9999999999999974465 ) ;
#5975 = ORIENTED_EDGE ( 'NONE', *, *, #16350, .T. ) ;
#5976 = CARTESIAN_POINT ( 'NONE',  ( -2.500000000000002220, 0.000000000000000000, 0.000000000000000000 ) ) ;
#5977 = CARTESIAN_POINT ( 'NONE',  ( -1.988169868018530906, 4.465502636338051445, -13.46874999795161543 ) ) ;
#5978 = ORIENTED_EDGE ( 'NONE', *, *, #4941, .T. ) ;
#5979 = CARTESIAN_POINT ( 'NONE',  ( 11.84374999795161365, -2.444050593750019651, 4.233219804643871598 ) ) ;
#5980 = EDGE_CURVE ( 'NONE', #17548, #19081, #1699, .T. ) ;
#5981 = LINE ( 'NONE', #7274, #7037 ) ;
#5982 = EDGE_CURVE ( 'NONE', #19487, #14187, #16264, .T. ) ;
#5983 = CARTESIAN_POINT ( 'NONE',  ( -7.937499999999998224, 0.7748640365313737011, -6.860966872759830281E-17 ) ) ;
#5984 = FACE_OUTER_BOUND ( 'NONE', #14049, .T. ) ;
#5985 = EDGE_CURVE ( 'NONE', #2730, #12192, #4693, .T. ) ;
#5986 = VERTEX_POINT ( 'NONE', #903 ) ;
#5987 = CIRCLE ( 'NONE', #13674, 1.000000000000004441 ) ;
#5988 = CARTESIAN_POINT ( 'NONE',  ( 2.790000000000000036, 24.22479935914659777, -2.133490293297098273 ) ) ;
#5989 = CYLINDRICAL_SURFACE ( 'NONE', #477, 0.9999999999999974465 ) ;
#5990 = CIRCLE ( 'NONE', #17187, 24.12539914357697768 ) ;
#5991 = ORIENTED_EDGE ( 'NONE', *, *, #4030, .F. ) ;
#5992 = EDGE_CURVE ( 'NONE', #8277, #12858, #3999, .T. ) ;
#5993 = LINE ( 'NONE', #4307, #8876 ) ;
#5994 = DIRECTION ( 'NONE',  ( -1.000000000000000000, 0.000000000000000000, -0.000000000000000000 ) ) ;
#5995 = CARTESIAN_POINT ( 'NONE',  ( 8.968749997951613651, -3.499494075959840966, 3.499494075959792116 ) ) ;
#5996 = CARTESIAN_POINT ( 'NONE',  ( 13.96874999795161365, 3.499494075959816541, 3.499494075959815653 ) ) ;
#5997 = LINE ( 'NONE', #17823, #6430 ) ;
#5998 = DIRECTION ( 'NONE',  ( 0.000000000000000000, 0.9510565162951498674, 0.3090169943749583870 ) ) ;
#5999 = ORIENTED_EDGE ( 'NONE', *, *, #14097, .T. ) ;
#6000 = CARTESIAN_POINT ( 'NONE',  ( -4.861323657744403448, 0.5109457054262118714, -13.84374999795161543 ) ) ;
#6001 = EDGE_CURVE ( 'NONE', #5891, #10126, #13631, .T. ) ;
#6002 = CARTESIAN_POINT ( 'NONE',  ( -2.000000000000001776, 0.000000000000000000, 0.000000000000000000 ) ) ;
#6003 = CIRCLE ( 'NONE', #8570, 5.200000000000000178 ) ;
#6004 = VERTEX_POINT ( 'NONE', #10020 ) ;
#6005 = PRODUCT_RELATED_PRODUCT_CATEGORY ( 'part', '', ( #3624 ) ) ;
#6006 = ADVANCED_FACE ( 'NONE', ( #19011 ), #6982, .F. ) ;
#6007 = CARTESIAN_POINT ( 'NONE',  ( -4.409619785863906571, 2.246813503491833508, -8.343749997951611874 ) ) ;
#6008 = CARTESIAN_POINT ( 'NONE',  ( 4.648860486681943627, -1.510506337161893864, -7.843749997951614539 ) ) ;
#6009 = ORIENTED_EDGE ( 'NONE', *, *, #14676, .F. ) ;
#6010 = CARTESIAN_POINT ( 'NONE',  ( 4.780397808154257078, -1.280903732194453859, -14.34374999795161365 ) ) ;
#6011 = CARTESIAN_POINT ( 'NONE',  ( 14.31249999590322552, -0.5958122406256373127, 5.668774803599156975 ) ) ;
#6012 = CARTESIAN_POINT ( 'NONE',  ( 4.366025403784385972, 7.562177826491085497, 37.99999999999999289 ) ) ;
#6013 = VERTEX_POINT ( 'NONE', #11601 ) ;
#6014 = FACE_BOUND ( 'NONE', #14414, .T. ) ;
#6015 = ORIENTED_EDGE ( 'NONE', *, *, #2581, .T. ) ;
#6016 = EDGE_CURVE ( 'NONE', #18366, #13534, #3410, .T. ) ;
#6018 = CARTESIAN_POINT ( 'NONE',  ( 0.000000000000000000, 0.000000000000000000, 29.00000000000000355 ) ) ;
#6017 = VECTOR ( 'NONE', #2825, 1000.000000000000000 ) ;
#6019 = ORIENTED_EDGE ( 'NONE', *, *, #18502, .F. ) ;
#6020 = DIRECTION ( 'NONE',  ( -1.000000000000000000, -0.000000000000000000, -0.000000000000000000 ) ) ;
#6021 = DIRECTION ( 'NONE',  ( 1.000000000000000000, 0.000000000000000000, 0.000000000000000000 ) ) ;
#6022 = DIRECTION ( 'NONE',  ( 1.000000000000000000, 0.000000000000000000, 0.000000000000000000 ) ) ;
#6023 = CARTESIAN_POINT ( 'NONE',  ( 6.468749997951615427, -4.233219804643904460, 2.444050593749960587 ) ) ;
#6024 = CARTESIAN_POINT ( 'NONE',  ( 13.00000000000000000, 4.333424887443004359, 2.261628166637590365 ) ) ;
#6025 = EDGE_CURVE ( 'NONE', #4362, #1514, #15874, .T. ) ;
#6026 = ORIENTED_EDGE ( 'NONE', *, *, #17169, .T. ) ;
#6027 = DIRECTION ( 'NONE',  ( 1.000000000000000000, 0.000000000000000000, 0.000000000000000000 ) ) ;
#6028 = CARTESIAN_POINT ( 'NONE',  ( -4.447186883680888769, -3.231070400981749025, -14.11718749948790830 ) ) ;
#6029 = EDGE_CURVE ( 'NONE', #6045, #17299, #5490, .T. ) ;
#6030 = AXIS2_PLACEMENT_3D ( 'NONE', #11468, #11561, #17762 ) ;
#6031 = EDGE_LOOP ( 'NONE', ( #5779, #2061, #6516, #4145, #8122, #6642 ) ) ;
#6032 = EDGE_CURVE ( 'NONE', #19214, #5836, #16409, .T. ) ;
#6033 = CARTESIAN_POINT ( 'NONE',  ( -11.00000000000000355, -4.898587196589412829E-16, 0.000000000000000000 ) ) ;
#6034 = CARTESIAN_POINT ( 'NONE',  ( 2.765633920072236851, -22.71065055754445439, -9.836394144775947979 ) ) ;
#6035 = VERTEX_POINT ( 'NONE', #14805 ) ;
#6036 = CARTESIAN_POINT ( 'NONE',  ( 2.999999999999998224, -3.950217066951263956, -3.681818181818183877 ) ) ;
#6037 = DIRECTION ( 'NONE',  ( 0.000000000000000000, 0.000000000000000000, -1.000000000000000000 ) ) ;
#6038 = CARTESIAN_POINT ( 'NONE',  ( -41.99999999999999289, -3.184081677783117402E-15, 0.000000000000000000 ) ) ;
#6039 = VERTEX_POINT ( 'NONE', #19394 ) ;
#6040 = SHAPE_REPRESENTATION ( 'DRIVER', ( #16724 ), #15776 ) ;
#6041 = CARTESIAN_POINT ( 'NONE',  ( 0.000000000000000000, -5.535312321042921369, 23.48180575137728354 ) ) ;
#6042 = DIRECTION ( 'NONE',  ( -0.9727768054256469288, -0.2317440114131819329, 5.551115123125782702E-17 ) ) ;
#6043 = CARTESIAN_POINT ( 'NONE',  ( 4.936344801571308061, 2.849999999999989431, -11.00000000000000711 ) ) ;
#6044 = SURFACE_SIDE_STYLE ('',( #10761 ) ) ;
#6045 = VERTEX_POINT ( 'NONE', #5682 ) ;
#6046 = ORIENTED_EDGE ( 'NONE', *, *, #9784, .T. ) ;
#6047 = CARTESIAN_POINT ( 'NONE',  ( -16.19790265903627713, 9.644882309621941374, 32.00000000000000000 ) ) ;
#6048 = CARTESIAN_POINT ( 'NONE',  ( 10.34374999795161543, 4.409619785863906571, -2.246813503491833508 ) ) ;
#6049 = ORIENTED_EDGE ( 'NONE', *, *, #10527, .F. ) ;
#6050 = ADVANCED_FACE ( 'NONE', ( #11506 ), #710, .T. ) ;
#6051 = CIRCLE ( 'NONE', #1591, 24.12539914357697413 ) ;
#6052 = CARTESIAN_POINT ( 'NONE',  ( 5.700000000000001066, -4.360680574150373717E-16, -12.66727757604273386 ) ) ;
#6053 = ORIENTED_EDGE ( 'NONE', *, *, #6407, .T. ) ;
#6054 = CARTESIAN_POINT ( 'NONE',  ( 16.11901729331276556, 5.562305898749055011, 35.00000000000000000 ) ) ;
#6055 = EDGE_CURVE ( 'NONE', #8859, #2783, #19104, .T. ) ;
#6056 = ORIENTED_EDGE ( 'NONE', *, *, #5606, .F. ) ;
#6057 = ADVANCED_FACE ( 'NONE', ( #17609 ), #3897, .F. ) ;
#6058 = DIRECTION ( 'NONE',  ( 0.000000000000000000, 0.000000000000000000, 1.000000000000000000 ) ) ;
#6059 = DIRECTION ( 'NONE',  ( 0.000000000000000000, -1.000000000000000000, 0.000000000000000000 ) ) ;
#6060 = CARTESIAN_POINT ( 'NONE',  ( 0.000000000000000000, 22.25075486061751207, -9.324097380959241121 ) ) ;
#6061 = AXIS2_PLACEMENT_3D ( 'NONE', #4728, #6404, #18435 ) ;
#6062 = VERTEX_POINT ( 'NONE', #4195 ) ;
#6063 = EDGE_CURVE ( 'NONE', #12858, #18724, #14597, .T. ) ;
#6064 = FACE_OUTER_BOUND ( 'NONE', #960, .T. ) ;
#6065 =( LENGTH_UNIT ( ) NAMED_UNIT ( * ) SI_UNIT ( .MILLI., .METRE. ) );
#6066 = VECTOR ( 'NONE', #15533, 1000.000000000000000 ) ;
#6067 = DIRECTION ( 'NONE',  ( 1.000000000000000000, 0.000000000000000000, 0.000000000000000000 ) ) ;
#6068 = ORIENTED_EDGE ( 'NONE', *, *, #18706, .T. ) ;
#6069 = CARTESIAN_POINT ( 'NONE',  ( 0.02436607992775934733, -21.30679549418640306, 12.59161484032904887 ) ) ;
#6070 = FACE_BOUND ( 'NONE', #16448, .T. ) ;
#6071 = CARTESIAN_POINT ( 'NONE',  ( 0.5321745326902582729, -26.83036154824997155, 3.467596033028195635 ) ) ;
#6072 = DIRECTION ( 'NONE',  ( 1.000000000000000000, 0.000000000000000000, 0.000000000000000000 ) ) ;
#6073 = CARTESIAN_POINT ( 'NONE',  ( -1.510506337161861667, 4.648860486681953397, -10.84374999795161543 ) ) ;
#6074 = ORIENTED_EDGE ( 'NONE', *, *, #2158, .T. ) ;
#6075 = PLANE ( 'NONE',  #4862 ) ;
#6076 = LINE ( 'NONE', #1491, #19375 ) ;
#6077 = AXIS2_PLACEMENT_3D ( 'NONE', #19095, #5389, #7067 ) ;
#6078 = EDGE_LOOP ( 'NONE', ( #15791, #1821, #5343, #13029, #14151 ) ) ;
#6079 = CARTESIAN_POINT ( 'NONE',  ( 2.765633920072235519, -18.55949924794880346, -16.37294372382878649 ) ) ;
#6080 = EDGE_CURVE ( 'NONE', #13634, #8711, #12352, .T. ) ;
#6081 = CARTESIAN_POINT ( 'NONE',  ( 7.843749997951614539, -4.781284448697200595, 1.016293382781377819 ) ) ;
#6082 = DIRECTION ( 'NONE',  ( 0.000000000000000000, 0.000000000000000000, 1.000000000000000000 ) ) ;
#6083 = CYLINDRICAL_SURFACE ( 'NONE', #15140, 13.20000000000000107 ) ;
#6084 = ORIENTED_EDGE ( 'NONE', *, *, #10386, .F. ) ;
#6085 = CYLINDRICAL_SURFACE ( 'NONE', #11713, 8.073750000000021743 ) ;
#6086 = SURFACE_STYLE_USAGE ( .BOTH. , #4401 ) ;
#6087 = CARTESIAN_POINT ( 'NONE',  ( -17.68117051311639898, -3.372863662543042818, -32.00000000000000000 ) ) ;
#6088 = DIRECTION ( 'NONE',  ( -0.000000000000000000, -0.000000000000000000, 1.000000000000000000 ) ) ;
#6089 = ORIENTED_EDGE ( 'NONE', *, *, #5484, .T. ) ;
#6090 = DIRECTION ( 'NONE',  ( 0.000000000000000000, 0.000000000000000000, 1.000000000000000000 ) ) ;
#6091 = AXIS2_PLACEMENT_3D ( 'NONE', #14906, #13598, #4394 ) ;
#6092 = CARTESIAN_POINT ( 'NONE',  ( -11.00000000000000355, 3.278623949159158446, -2.625000000000002220 ) ) ;
#6093 = CARTESIAN_POINT ( 'NONE',  ( 12.46874999795161543, -4.648860486681943627, -1.510506337161893642 ) ) ;
#6094 = EDGE_CURVE ( 'NONE', #8225, #10153, #6076, .T. ) ;
#6095 = EDGE_CURVE ( 'NONE', #10294, #3268, #3760, .T. ) ;
#6096 = EDGE_LOOP ( 'NONE', ( #5791, #16844, #1405, #1622 ) ) ;
#6097 = CYLINDRICAL_SURFACE ( 'NONE', #15080, 12.00000000000000178 ) ;
#6098 = CARTESIAN_POINT ( 'NONE',  ( 1.988169868018593300, 4.465502636338024800, -9.843749997951615427 ) ) ;
#6099 = VERTEX_POINT ( 'NONE', #6177 ) ;
#6100 = CARTESIAN_POINT ( 'NONE',  ( 9.843749997951615427, -3.954556930911881985, 2.873153789725797491 ) ) ;
#6101 = CARTESIAN_POINT ( 'NONE',  ( 2.299999999999998490, 0.000000000000000000, 0.000000000000000000 ) ) ;
#6102 = EDGE_LOOP ( 'NONE', ( #19557, #3229, #16922, #497 ) ) ;
#6103 = EDGE_CURVE ( 'NONE', #13819, #4366, #12680, .T. ) ;
#6104 = ADVANCED_FACE ( 'NONE', ( #9199 ), #12195, .T. ) ;
#6105 = CIRCLE ( 'NONE', #5774, 24.12539914357697768 ) ;
#6106 = AXIS2_PLACEMENT_3D ( 'NONE', #11383, #6953, #14587 ) ;
#6107 = CIRCLE ( 'NONE', #9971, 9.000000000000001776 ) ;
#6108 = DIRECTION ( 'NONE',  ( 0.000000000000000000, 0.000000000000000000, 1.000000000000000000 ) ) ;
#6109 = DIRECTION ( 'NONE',  ( 0.000000000000000000, 0.000000000000000000, -1.000000000000000000 ) ) ;
#6110 = ORIENTED_EDGE ( 'NONE', *, *, #8375, .F. ) ;
#6111 = B_SPLINE_CURVE_WITH_KNOTS ( 'NONE', 3,
 ( #19179, #2378, #11584, #7057, #16288, #11489, #12894, #11680 ),
 .UNSPECIFIED., .F., .F.,
 ( 4, 2, 2, 4 ),
 ( 0.004637198101876887496, 0.005792104118025196563, 0.006947010134173506497, 0.009256822166470123764 ),
 .UNSPECIFIED. ) ;
#6112 = DIRECTION ( 'NONE',  ( 0.000000000000000000, 0.000000000000000000, -1.000000000000000000 ) ) ;
#6113 = CARTESIAN_POINT ( 'NONE',  ( -1.510506337161861667, 4.648860486681953397, -10.46874999795161720 ) ) ;
#6114 = ORIENTED_EDGE ( 'NONE', *, *, #18465, .T. ) ;
#6115 = DIRECTION ( 'NONE',  ( 1.000000000000000000, 3.873737557103174326E-15, 0.000000000000000000 ) ) ;
#6116 = ORIENTED_EDGE ( 'NONE', *, *, #1443, .F. ) ;
#6117 = CARTESIAN_POINT ( 'NONE',  ( 2.789999999999999147, -20.62201879784904079, -12.52067188844374179 ) ) ;
#6118 = VERTEX_POINT ( 'NONE', #16902 ) ;
#6119 = FACE_OUTER_BOUND ( 'NONE', #17380, .T. ) ;
#6120 = CARTESIAN_POINT ( 'NONE',  ( -2.000000000000001776, 9.674709713264090115E-16, 7.800000000000000711 ) ) ;
#6121 = CARTESIAN_POINT ( 'NONE',  ( 2.789999999999999147, -24.04302995059966719, 1.991882183130210482 ) ) ;
#6122 = AXIS2_PLACEMENT_3D ( 'NONE', #14644, #7009, #13133 ) ;
#6123 = CIRCLE ( 'NONE', #11238, 7.174999999999998934 ) ;
#6124 = CARTESIAN_POINT ( 'NONE',  ( 2.718131885465890463, 18.89333555428578748, -16.91241718341978029 ) ) ;
#6125 = ORIENTED_EDGE ( 'NONE', *, *, #6631, .F. ) ;
#6126 = CIRCLE ( 'NONE', #16040, 4.000000000000000000 ) ;
#6127 = LINE ( 'NONE', #12149, #16072 ) ;
#6128 = DIRECTION ( 'NONE',  ( 0.000000000000000000, 0.000000000000000000, 1.000000000000000000 ) ) ;
#6129 = EDGE_CURVE ( 'NONE', #11459, #9163, #6584, .T. ) ;
#6130 = ADVANCED_FACE ( 'NONE', ( #4588 ), #5883, .T. ) ;
#6131 = LINE ( 'NONE', #10748, #10009 ) ;
#6132 = CARTESIAN_POINT ( 'NONE',  ( 16.19790265903627358, 9.644882309621939598, 32.00000000000000000 ) ) ;
#6133 = DIRECTION ( 'NONE',  ( 1.000000000000000000, 0.000000000000000000, 0.000000000000000000 ) ) ;
#6134 = ORIENTED_EDGE ( 'NONE', *, *, #3631, .F. ) ;
#6135 = VECTOR ( 'NONE', #4596, 1000.000000000000000 ) ;
#6136 = CARTESIAN_POINT ( 'NONE',  ( 6.000000000000005329, -4.936344801571327601, 2.849999999999954348 ) ) ;
#6137 = CARTESIAN_POINT ( 'NONE',  ( 3.846120219227923798, -3.114526743279282250, -11.96874999795161365 ) ) ;
#6138 = VECTOR ( 'NONE', #14609, 1000.000000000000000 ) ;
#6139 = ORIENTED_EDGE ( 'NONE', *, *, #7571, .T. ) ;
#6140 = EDGE_CURVE ( 'NONE', #5140, #15581, #2075, .T. ) ;
#6141 = ORIENTED_EDGE ( 'NONE', *, *, #4599, .F. ) ;
#6142 = APPLICATION_PROTOCOL_DEFINITION ( 'draft international standard', 'automotive_design', 1998, #11110 ) ;
#6143 = CARTESIAN_POINT ( 'NONE',  ( -5.207209108562804722, 2.318398865532109276, -14.00000000000000533 ) ) ;
#6144 = DIRECTION ( 'NONE',  ( -0.000000000000000000, -0.000000000000000000, 1.000000000000000000 ) ) ;
#6145 = ORIENTED_EDGE ( 'NONE', *, *, #14267, .T. ) ;
#6146 = EDGE_LOOP ( 'NONE', ( #19663, #330 ) ) ;
#6147 = LINE ( 'NONE', #7649, #7932 ) ;
#6148 = EDGE_CURVE ( 'NONE', #11483, #17227, #18104, .T. ) ;
#6149 = CARTESIAN_POINT ( 'NONE',  ( 12.84374999795161543, 4.648860486681953397, 1.510506337161861223 ) ) ;
#6150 = EDGE_CURVE ( 'NONE', #4659, #7585, #16807, .T. ) ;
#6151 = ORIENTED_EDGE ( 'NONE', *, *, #10432, .F. ) ;
#6152 = VECTOR ( 'NONE', #14884, 1000.000000000000000 ) ;
#6153 = ORIENTED_EDGE ( 'NONE', *, *, #1271, .T. ) ;
#6154 = SURFACE_STYLE_FILL_AREA ( #60 ) ;
#6155 = ORIENTED_EDGE ( 'NONE', *, *, #4649, .T. ) ;
#6156 = AXIS2_PLACEMENT_3D ( 'NONE', #17148, #17343, #9548 ) ;
#6157 = STYLED_ITEM ( 'NONE', ( #3595 ), #3136 ) ;
#6158 =( BOUNDED_SURFACE ( )  B_SPLINE_SURFACE ( 1, 2, ( 
 ( #19258, #958, #7036, #16269, #17473, #17672, #4156, #8369, #11472, #10078, #1059, #5455, #13167, #16177, #14482, #5359, #8760 ),
 ( #14577, #3765, #14864, #9885, #19065, #772, #11661, #2447, #18968, #6745, #8472, #13265, #17573, #11565, #19355, #3859, #4059 ) ),
 .UNSPECIFIED., .F., .F., .F. ) 
 B_SPLINE_SURFACE_WITH_KNOTS ( ( 2, 2 ),
 ( 3, 2, 2, 2, 2, 2, 2, 2, 3 ),
 ( 0.000000000000000000, 1.000000000000000000 ),
 ( 0.000000000000000000, 0.05000000000000000278, 0.1000000000000000056, 0.1499999999999999944, 0.2000000000000000111, 0.2500000000000000000, 0.2999999999999999889, 0.3499999999999999778, 0.4000000000000000222 ),
 .UNSPECIFIED. ) 
 GEOMETRIC_REPRESENTATION_ITEM ( )  RATIONAL_B_SPLINE_SURFACE ( (
 ( 1.000000000000000000, 0.9876883405951377704, 1.000000000000000000, 0.9876883405951377704, 1.000000000000000000, 0.9876883405951377704, 1.000000000000000000, 0.9876883405951377704, 1.000000000000000000, 0.9876883405951377704, 1.000000000000000000, 0.9876883405951377704, 1.000000000000000000, 0.9876883405951377704, 1.000000000000000000, 0.9876883405951377704, 1.000000000000000000),
 ( 1.000000000000000000, 0.9876883405951377704, 1.000000000000000000, 0.9876883405951377704, 1.000000000000000000, 0.9876883405951377704, 1.000000000000000000, 0.9876883405951377704, 1.000000000000000000, 0.9876883405951377704, 1.000000000000000000, 0.9876883405951377704, 1.000000000000000000, 0.9876883405951377704, 1.000000000000000000, 0.9876883405951377704, 1.000000000000000000) ) ) 
 REPRESENTATION_ITEM ( '' )  SURFACE ( )  );
#6159 = CARTESIAN_POINT ( 'NONE',  ( 0.000000000000000000, 4.898587196589412829E-16, -4.000000000000000000 ) ) ;
#6160 = DIRECTION ( 'NONE',  ( 0.000000000000000000, 1.000000000000000000, -1.224646799147353207E-16 ) ) ;
#6161 = CARTESIAN_POINT ( 'NONE',  ( 4.611396867937178179, -3.350375938067129855, -9.312499995903225525 ) ) ;
#6162 = CIRCLE ( 'NONE', #4248, 4.400000000000001243 ) ;
#6163 = ORIENTED_EDGE ( 'NONE', *, *, #1499, .F. ) ;
#6164 = ORIENTED_EDGE ( 'NONE', *, *, #6233, .F. ) ;
#6165 = LINE ( 'NONE', #19773, #6595 ) ;
#6166 = PRESENTATION_STYLE_ASSIGNMENT (( #16492 ) ) ;
#6167 = CARTESIAN_POINT ( 'NONE',  ( 1.039999999999996039, 24.89775460606832169, 12.96210679857795256 ) ) ;
#6168 = EDGE_LOOP ( 'NONE', ( #8836, #19763, #1398, #2756 ) ) ;
#6169 = DIRECTION ( 'NONE',  ( -1.000000000000000000, 1.224646799147353207E-16, 0.000000000000000000 ) ) ;
#6170 = CARTESIAN_POINT ( 'NONE',  ( 4.476417968967386862, 17.43449690031536292, 35.00000000000000000 ) ) ;
#6171 = CARTESIAN_POINT ( 'NONE',  ( -5.700000000000000178, -2.180340287075187351E-16, -12.66727757604271076 ) ) ;
#6172 = VECTOR ( 'NONE', #4597, 1000.000000000000000 ) ;
#6173 = CARTESIAN_POINT ( 'NONE',  ( 2.632969638839692372, 22.37100459959346566, 12.81671916049022641 ) ) ;
#6174 = CARTESIAN_POINT ( 'NONE',  ( 3.499494075959815653, 3.499494075959816541, -13.96874999795161365 ) ) ;
#6175 = ORIENTED_EDGE ( 'NONE', *, *, #385, .F. ) ;
#6176 = DIRECTION ( 'NONE',  ( 0.000000000000000000, 0.000000000000000000, 1.000000000000000000 ) ) ;
#6177 = CARTESIAN_POINT ( 'NONE',  ( 1.039999999999996705, -20.02152543075331081, -19.67366047555552555 ) ) ;
#6178 = VERTEX_POINT ( 'NONE', #1195 ) ;
#6179 = DIRECTION ( 'NONE',  ( 7.654042494670960318E-17, 0.6250000000000002220, -0.7806247497997995666 ) ) ;
#6180 = CARTESIAN_POINT ( 'NONE',  ( 0.5321745227542252765, -19.66801664102716884, 18.57583492944412384 ) ) ;
#6181 = CARTESIAN_POINT ( 'NONE',  ( 1.039999999999997371, 25.12109765559653596, 12.52377138324232675 ) ) ;
#6182 = CARTESIAN_POINT ( 'NONE',  ( -1.000000000000001998, 18.00000000000000355, -35.00000000000000000 ) ) ;
#6183 = VERTEX_POINT ( 'NONE', #11998 ) ;
#6184 = CARTESIAN_POINT ( 'NONE',  ( 14.00000000000000533, 3.350375938067097881, 4.611396867937200383 ) ) ;
#6185 = CARTESIAN_POINT ( 'NONE',  ( 0.000000000000000000, 0.000000000000000000, 32.00000000000000000 ) ) ;
#6186 = FACE_OUTER_BOUND ( 'NONE', #6911, .T. ) ;
#6187 = ORIENTED_EDGE ( 'NONE', *, *, #9883, .F. ) ;
#6188 = FACE_BOUND ( 'NONE', #3936, .T. ) ;
#6189 = MECHANICAL_DESIGN_GEOMETRIC_PRESENTATION_REPRESENTATION (  '', ( #1091 ), #461 ) ;
#6190 = AXIS2_PLACEMENT_3D ( 'NONE', #10147, #16245, #8636 ) ;
#6191 = CARTESIAN_POINT ( 'NONE',  ( 14.84374999795161543, -4.861323657744410554, 0.5109457054261454800 ) ) ;
#6192 = CARTESIAN_POINT ( 'NONE',  ( 3.814044456245474279, -4.235925505221167064, -12.00000000000000533 ) ) ;
#6193 = EDGE_CURVE ( 'NONE', #10924, #6045, #548, .T. ) ;
#6194 = DIRECTION ( 'NONE',  ( 1.000000000000000000, 0.000000000000000000, 0.000000000000000000 ) ) ;
#6195 = ORIENTED_EDGE ( 'NONE', *, *, #977, .F. ) ;
#6196 = CARTESIAN_POINT ( 'NONE',  ( -12.32184790671639085, 13.12143529358541549, 32.00000000000000000 ) ) ;
#6197 = DIRECTION ( 'NONE',  ( -1.000000000000000000, -0.000000000000000000, 0.000000000000000000 ) ) ;
#6198 = ORIENTED_EDGE ( 'NONE', *, *, #16620, .F. ) ;
#6199 = AXIS2_PLACEMENT_3D ( 'NONE', #8518, #6895, #3811 ) ;
#6200 = DIRECTION ( 'NONE',  ( 1.000000000000000000, 6.419766481290786633E-33, -0.000000000000000000 ) ) ;
#6201 = EDGE_LOOP ( 'NONE', ( #11466, #3863, #19502, #12108 ) ) ;
#6202 = AXIS2_PLACEMENT_3D ( 'NONE', #4949, #8034, #452 ) ;
#6203 = DIRECTION ( 'NONE',  ( 0.000000000000000000, 0.000000000000000000, -1.000000000000000000 ) ) ;
#6204 = EDGE_CURVE ( 'NONE', #17967, #123, #3085, .T. ) ;
#6205 = CARTESIAN_POINT ( 'NONE',  ( -5.700000000000001066, 0.000000000000000000, -6.656249997951614539 ) ) ;
#6206 = EDGE_LOOP ( 'NONE', ( #3046, #11436, #5600, #6318 ) ) ;
#6207 = CARTESIAN_POINT ( 'NONE',  ( -25.31088913245550032, 24.69615242270646149, 41.99999999999999289 ) ) ;
#6208 = CYLINDRICAL_SURFACE ( 'NONE', #8451, 13.19999999999999929 ) ;
#6209 = ORIENTED_EDGE ( 'NONE', *, *, #1255, .F. ) ;
#6210 = CARTESIAN_POINT ( 'NONE',  ( 2.789999999999999147, 15.04425356660760293, 20.70663861606276868 ) ) ;
#6211 = EDGE_LOOP ( 'NONE', ( #14715, #7305 ) ) ;
#6212 = CARTESIAN_POINT ( 'NONE',  ( 4.484949146646356688, -3.631840208645826351, -12.81249999590322552 ) ) ;
#6213 = VERTEX_POINT ( 'NONE', #4293 ) ;
#6214 = EDGE_CURVE ( 'NONE', #13293, #16711, #8333, .T. ) ;
#6215 = DIRECTION ( 'NONE',  ( 1.000000000000000000, 0.000000000000000000, 0.000000000000000000 ) ) ;
#6216 = FACE_OUTER_BOUND ( 'NONE', #1627, .T. ) ;
#6217 =( GEOMETRIC_REPRESENTATION_CONTEXT ( 3 ) GLOBAL_UNCERTAINTY_ASSIGNED_CONTEXT ( ( #5388 ) ) GLOBAL_UNIT_ASSIGNED_CONTEXT ( ( #9778, #1242, #10261 ) ) REPRESENTATION_CONTEXT ( 'NONE', 'WORKASPACE' ) );
#6218 = CARTESIAN_POINT ( 'NONE',  ( 7.468749997951615427, 4.781284448697194378, -1.016293382781411125 ) ) ;
#6219 = EDGE_LOOP ( 'NONE', ( #1030, #727 ) ) ;
#6220 = DIRECTION ( 'NONE',  ( 0.000000000000000000, 0.000000000000000000, 1.000000000000000000 ) ) ;
#6221 = CARTESIAN_POINT ( 'NONE',  ( -41.99999999999999289, 4.999999999999998224, 5.000000000000000000 ) ) ;
#6222 = ORIENTED_EDGE ( 'NONE', *, *, #13671, .T. ) ;
#6223 = CARTESIAN_POINT ( 'NONE',  ( -13.32184790671639618, 13.12143529358541549, 35.00000000000000000 ) ) ;
#6224 = EDGE_CURVE ( 'NONE', #8313, #9186, #15497, .T. ) ;
#6225 = DIRECTION ( 'NONE',  ( -1.000000000000000000, 1.224646799147353207E-16, 0.000000000000000000 ) ) ;
#6226 = ORIENTED_EDGE ( 'NONE', *, *, #16665, .T. ) ;
#6227 = VECTOR ( 'NONE', #11089, 1000.000000000000000 ) ;
#6228 = DIRECTION ( 'NONE',  ( 0.000000000000000000, 0.000000000000000000, -1.000000000000000000 ) ) ;
#6229 = DIRECTION ( 'NONE',  ( -1.000000000000000000, 1.224646799147353207E-16, 0.000000000000000000 ) ) ;
#6230 = DIRECTION ( 'NONE',  ( 1.000000000000000000, 0.000000000000000000, 0.000000000000000000 ) ) ;
#6231 = ORIENTED_EDGE ( 'NONE', *, *, #6249, .F. ) ;
#6232 = DIRECTION ( 'NONE',  ( 0.000000000000000000, 0.000000000000000000, 1.000000000000000000 ) ) ;
#6233 = EDGE_CURVE ( 'NONE', #4149, #11016, #13994, .T. ) ;
#6234 = EDGE_LOOP ( 'NONE', ( #11776, #7666, #2306, #3265 ) ) ;
#6235 = ITEM_DEFINED_TRANSFORMATION ( 'NONE', 'NONE', #930,  #16724 ) ;
#6236 = DIRECTION ( 'NONE',  ( -0.8660254037844382635, -0.5000000000000005551, 0.000000000000000000 ) ) ;
#6237 = DIRECTION ( 'NONE',  ( -1.000000000000000000, -0.000000000000000000, -0.000000000000000000 ) ) ;
#6238 = ORIENTED_EDGE ( 'NONE', *, *, #18421, .T. ) ;
#6239 = ORIENTED_EDGE ( 'NONE', *, *, #8236, .F. ) ;
#6240 = EDGE_CURVE ( 'NONE', #14128, #1723, #5638, .T. ) ;
#6241 = DIRECTION ( 'NONE',  ( -0.000000000000000000, -0.000000000000000000, 1.000000000000000000 ) ) ;
#6242 = CARTESIAN_POINT ( 'NONE',  ( 1.749999999999998002, 0.000000000000000000, 0.000000000000000000 ) ) ;
#6243 = EDGE_LOOP ( 'NONE', ( #7704, #4746, #1373, #11983 ) ) ;
#6244 = CIRCLE ( 'NONE', #192, 3.323499999999993015 ) ;
#6245 = AXIS2_PLACEMENT_3D ( 'NONE', #1315, #3009, #7392 ) ;
#6246 = DIRECTION ( 'NONE',  ( 1.000000000000000000, 0.000000000000000000, 0.000000000000000000 ) ) ;
#6247 = ADVANCED_FACE ( 'NONE', ( #14082 ), #3482, .F. ) ;
#6248 = VERTEX_POINT ( 'NONE', #11289 ) ;
#6249 = EDGE_CURVE ( 'NONE', #10962, #14651, #2829, .T. ) ;
#6250 = EDGE_CURVE ( 'NONE', #4659, #5172, #7548, .T. ) ;
#6251 = DIRECTION ( 'NONE',  ( 1.000000000000000000, 0.000000000000000000, 0.000000000000000000 ) ) ;
#6252 = CARTESIAN_POINT ( 'NONE',  ( 8.343749997951613651, 2.695436003842704764, 4.150607464521811174 ) ) ;
#6253 = LINE ( 'NONE', #18187, #4005 ) ;
#6254 = AXIS2_PLACEMENT_3D ( 'NONE', #16936, #18524, #14119 ) ;
#6255 = ORIENTED_EDGE ( 'NONE', *, *, #11780, .F. ) ;
#6256 = ORIENTED_EDGE ( 'NONE', *, *, #16644, .F. ) ;
#6257 = DIRECTION ( 'NONE',  ( 0.000000000000000000, 0.000000000000000000, -1.000000000000000000 ) ) ;
#6258 = DIRECTION ( 'NONE',  ( -1.000000000000000000, -0.000000000000000000, -0.000000000000000000 ) ) ;
#6259 = VECTOR ( 'NONE', #1371, 1000.000000000000114 ) ;
#6260 = EDGE_LOOP ( 'NONE', ( #5928, #13945 ) ) ;
#6261 = ORIENTED_EDGE ( 'NONE', *, *, #10207, .T. ) ;
#6262 = CARTESIAN_POINT ( 'NONE',  ( -11.00000000000000355, 3.278623949159158446, -2.625000000000002220 ) ) ;
#6263 = CARTESIAN_POINT ( 'NONE',  ( 1.185096637661176677, -5.575441324182703440, -8.312499995903225525 ) ) ;
#6264 = ADVANCED_FACE ( 'NONE', ( #9590 ), #7873, .F. ) ;
#6265 = CARTESIAN_POINT ( 'NONE',  ( -15.00000000000000355, -4.400000000000000355, 5.388445916248354013E-16 ) ) ;
#6266 = DIRECTION ( 'NONE',  ( 1.000000000000000000, 0.000000000000000000, 0.000000000000000000 ) ) ;
#6267 = CARTESIAN_POINT ( 'NONE',  ( 4.080749450109649956, 4.080749450109650844, -13.50000000000000533 ) ) ;
#6268 = EDGE_LOOP ( 'NONE', ( #4752, #10576, #6415, #1254 ) ) ;
#6269 = CARTESIAN_POINT ( 'NONE',  ( 8.343749997951611874, -2.695436003842674566, -4.150607464521828938 ) ) ;
#6270 = EDGE_CURVE ( 'NONE', #2987, #3123, #15882, .T. ) ;
#6271 =( BOUNDED_SURFACE ( )  B_SPLINE_SURFACE ( 1, 2, ( 
 ( #8141, #10853, #3639, #11048, #17154, #6622, #448, #2038, #12654, #1747, #16959, #9556, #6524, #13952, #1937, #9761, #13854 ),
 ( #11151, #17351, #3538, #3444, #243, #1645, #10952, #147, #17058, #18846, #554, #17248, #12452, #12358, #7935, #4743, #9656 ) ),
 .UNSPECIFIED., .F., .F., .F. ) 
 B_SPLINE_SURFACE_WITH_KNOTS ( ( 2, 2 ),
 ( 3, 2, 2, 2, 2, 2, 2, 2, 3 ),
 ( 0.000000000000000000, 1.000000000000000000 ),
 ( 0.000000000000000000, 0.05000000000000000278, 0.1000000000000000056, 0.1499999999999999944, 0.2000000000000000111, 0.2500000000000000000, 0.2999999999999999889, 0.3499999999999999778, 0.4000000000000000222 ),
 .UNSPECIFIED. ) 
 GEOMETRIC_REPRESENTATION_ITEM ( )  RATIONAL_B_SPLINE_SURFACE ( (
 ( 1.000000000000000000, 0.9876883405951377704, 1.000000000000000000, 0.9876883405951377704, 1.000000000000000000, 0.9876883405951377704, 1.000000000000000000, 0.9876883405951377704, 1.000000000000000000, 0.9876883405951377704, 1.000000000000000000, 0.9876883405951377704, 1.000000000000000000, 0.9876883405951377704, 1.000000000000000000, 0.9876883405951377704, 1.000000000000000000),
 ( 1.000000000000000000, 0.9876883405951377704, 1.000000000000000000, 0.9876883405951377704, 1.000000000000000000, 0.9876883405951377704, 1.000000000000000000, 0.9876883405951377704, 1.000000000000000000, 0.9876883405951377704, 1.000000000000000000, 0.9876883405951377704, 1.000000000000000000, 0.9876883405951377704, 1.000000000000000000, 0.9876883405951377704, 1.000000000000000000) ) ) 
 REPRESENTATION_ITEM ( '' )  SURFACE ( )  );
#6272 = DIRECTION ( 'NONE',  ( 0.8660254037844382635, 0.5000000000000005551, 0.000000000000000000 ) ) ;
#6273 = AXIS2_PLACEMENT_3D ( 'NONE', #4795, #18309, #13703 ) ;
#6274 = ORIENTED_EDGE ( 'NONE', *, *, #14703, .F. ) ;
#6275 = CARTESIAN_POINT ( 'NONE',  ( 10.00000000000000533, 1.185096637661293251, -5.575441324182679459 ) ) ;
#6276 = CARTESIAN_POINT ( 'NONE',  ( 13.84374999795161543, 0.5109457054262118714, -4.861323657744403448 ) ) ;
#6277 = EDGE_CURVE ( 'NONE', #2859, #5462, #17797, .T. ) ;
#6278 = DIRECTION ( 'NONE',  ( -1.000000000000000000, 0.000000000000000000, 0.000000000000000000 ) ) ;
#6279 = LINE ( 'NONE', #12404, #7132 ) ;
#6280 = ORIENTED_EDGE ( 'NONE', *, *, #12876, .T. ) ;
#6281 = CARTESIAN_POINT ( 'NONE',  ( 14.46874999795161720, 2.873153789725825913, 3.954556930911861112 ) ) ;
#6282 = CARTESIAN_POINT ( 'NONE',  ( 0.7592463896980037319, 19.12676442129342647, 19.86438386685667368 ) ) ;
#6283 = VERTEX_POINT ( 'NONE', #15687 ) ;
#6284 = DIRECTION ( 'NONE',  ( 0.000000000000000000, 0.000000000000000000, 1.000000000000000000 ) ) ;
#6285 = VECTOR ( 'NONE', #10392, 1000.000000000000000 ) ;
#6286 = FACE_OUTER_BOUND ( 'NONE', #4487, .T. ) ;
#6287 = CARTESIAN_POINT ( 'NONE',  ( 3.143139765844590983, -4.840010801796506001, -12.50000000000000533 ) ) ;
#6288 = VECTOR ( 'NONE', #9969, 1000.000000000000000 ) ;
#6289 = DIRECTION ( 'NONE',  ( 0.000000000000000000, 0.000000000000000000, -1.000000000000000000 ) ) ;
#6290 = VERTEX_POINT ( 'NONE', #1690 ) ;
#6291 = CARTESIAN_POINT ( 'NONE',  ( 2.790000000000076863, -23.69897269326681055, 5.456611084821764379 ) ) ;
#6292 = CARTESIAN_POINT ( 'NONE',  ( 0.000000000000000000, 0.000000000000000000, 35.00000000000000000 ) ) ;
#6293 = ORIENTED_EDGE ( 'NONE', *, *, #2059, .F. ) ;
#6294 = CARTESIAN_POINT ( 'NONE',  ( -30.00000000000000000, 1.224646799147352468E-16, 0.000000000000000000 ) ) ;
#6295 = EDGE_CURVE ( 'NONE', #12478, #6099, #16507, .T. ) ;
#6296 = CARTESIAN_POINT ( 'NONE',  ( 0.000000000000000000, 12.52067188844351442, 20.62201879784919001 ) ) ;
#6297 = ORIENTED_EDGE ( 'NONE', *, *, #8769, .T. ) ;
#6298 = CIRCLE ( 'NONE', #7573, 5.700000000000001954 ) ;
#6299 = EDGE_CURVE ( 'NONE', #8343, #4507, #8525, .T. ) ;
#6300 = CIRCLE ( 'NONE', #17505, 1.000000000000000888 ) ;
#6301 = CARTESIAN_POINT ( 'NONE',  ( 2.031033479673592268, -19.86422722021325882, 19.12621924769859660 ) ) ;
#6302 = CARTESIAN_POINT ( 'NONE',  ( 11.50000000000000355, -3.631840208645826351, 4.484949146646356688 ) ) ;
#6303 = ORIENTED_EDGE ( 'NONE', *, *, #18715, .F. ) ;
#6304 = DIRECTION ( 'NONE',  ( 0.000000000000000000, 0.000000000000000000, -1.000000000000000000 ) ) ;
#6305 = CARTESIAN_POINT ( 'NONE',  ( 0.1855654851361731306, 23.63475234378982748, 10.67816411292173306 ) ) ;
#6306 = ORIENTED_EDGE ( 'NONE', *, *, #4691, .T. ) ;
#6307 = DIRECTION ( 'NONE',  ( -1.000000000000000000, -0.000000000000000000, -0.000000000000000000 ) ) ;
#6308 = ORIENTED_EDGE ( 'NONE', *, *, #5484, .F. ) ;
#6309 = DIRECTION ( 'NONE',  ( -1.000000000000000000, -0.000000000000000000, -0.000000000000000000 ) ) ;
#6310 = ORIENTED_EDGE ( 'NONE', *, *, #12373, .T. ) ;
#6311 = EDGE_CURVE ( 'NONE', #7195, #3069, #1166, .T. ) ;
#6312 = DIRECTION ( 'NONE',  ( 0.000000000000000000, 0.000000000000000000, -1.000000000000000000 ) ) ;
#6313 = DIRECTION ( 'NONE',  ( 1.000000000000000000, 0.000000000000000000, 0.000000000000000000 ) ) ;
#6314 = CARTESIAN_POINT ( 'NONE',  ( 3.114526743279282694, 3.846120219227923798, -6.968749997951614539 ) ) ;
#6315 = AXIS2_PLACEMENT_3D ( 'NONE', #5293, #11592, #3691 ) ;
#6316 = CARTESIAN_POINT ( 'NONE',  ( 1.280903732194421663, -4.780397808154265960, -13.96874999795161365 ) ) ;
#6317 = TOROIDAL_SURFACE ( 'NONE', #2172, 24.12539914357697768, 8.000000000000000000 ) ;
#6318 = ORIENTED_EDGE ( 'NONE', *, *, #12966, .T. ) ;
#6319 = CARTESIAN_POINT ( 'NONE',  ( 6.000000000000005329, 0.000000000000000000, 0.000000000000000000 ) ) ;
#6320 = CARTESIAN_POINT ( 'NONE',  ( 1.039999999999997593, 0.000000000000000000, 0.000000000000000000 ) ) ;
#6321 = VERTEX_POINT ( 'NONE', #11186 ) ;
#6322 = EDGE_CURVE ( 'NONE', #5554, #17466, #17286, .T. ) ;
#6323 = CARTESIAN_POINT ( 'NONE',  ( 1.749999999999998002, 4.147968289691672084, -27.76164181293047406 ) ) ;
#6324 = CARTESIAN_POINT ( 'NONE',  ( 15.19790265903627358, 9.644882309621939598, -32.00000000000000000 ) ) ;
#6325 = VECTOR ( 'NONE', #4776, 1000.000000000000000 ) ;
#6326 = VERTEX_POINT ( 'NONE', #2076 ) ;
#6327 = CARTESIAN_POINT ( 'NONE',  ( 0.000000000000000000, 0.000000000000000000, 0.000000000000000000 ) ) ;
#6328 = FACE_OUTER_BOUND ( 'NONE', #9235, .T. ) ;
#6329 = EDGE_LOOP ( 'NONE', ( #19166, #3815, #15696, #6019 ) ) ;
#6330 = DIRECTION ( 'NONE',  ( 1.000000000000000000, 0.000000000000000000, 0.000000000000000000 ) ) ;
#6331 = ORIENTED_EDGE ( 'NONE', *, *, #9263, .F. ) ;
#6332 = PRODUCT_CONTEXT ( 'NONE', #19395, 'mechanical' ) ;
#6333 = PLANE ( 'NONE',  #14479 ) ;
#6334 = CARTESIAN_POINT ( 'NONE',  ( 13.46874999795161543, -0.5109457054261780096, 4.861323657744406113 ) ) ;
#6335 = ORIENTED_EDGE ( 'NONE', *, *, #8508, .F. ) ;
#6336 = ORIENTED_EDGE ( 'NONE', *, *, #13205, .T. ) ;
#6337 = CARTESIAN_POINT ( 'NONE',  ( -19.00000000000000355, 1.224646799147353207E-16, 0.000000000000000000 ) ) ;
#6338 = CARTESIAN_POINT ( 'NONE',  ( 2.695436003842732298, 4.150607464521792522, -10.34374999795161543 ) ) ;
#6339 = ORIENTED_EDGE ( 'NONE', *, *, #6539, .F. ) ;
#6340 = EDGE_CURVE ( 'NONE', #2660, #5462, #3794, .T. ) ;
#6341 = EDGE_CURVE ( 'NONE', #18865, #3717, #5452, .T. ) ;
#6342 = CIRCLE ( 'NONE', #16907, 6.543750000000023270 ) ;
#6343 = CARTESIAN_POINT ( 'NONE',  ( -4.476417968967385974, 17.43449690031536292, 32.00000000000000000 ) ) ;
#6344 = EDGE_LOOP ( 'NONE', ( #19742, #9446, #9633, #18836 ) ) ;
#6345 = AXIS2_PLACEMENT_3D ( 'NONE', #19552, #13660, #8763 ) ;
#6346 = DIRECTION ( 'NONE',  ( -0.000000000000000000, -0.000000000000000000, 1.000000000000000000 ) ) ;
#6347 = LINE ( 'NONE', #7857, #9353 ) ;
#6348 = FACE_BOUND ( 'NONE', #13390, .T. ) ;
#6349 = VECTOR ( 'NONE', #5450, 1000.000000000000000 ) ;
#6350 = ORIENTED_EDGE ( 'NONE', *, *, #12629, .T. ) ;
#6351 = DIRECTION ( 'NONE',  ( 0.000000000000000000, 0.000000000000000000, 1.000000000000000000 ) ) ;
#6352 = DIRECTION ( 'NONE',  ( 1.000000000000000000, 0.000000000000000000, 0.000000000000000000 ) ) ;
#6353 = ORIENTED_EDGE ( 'NONE', *, *, #10065, .F. ) ;
#6354 = ORIENTED_EDGE ( 'NONE', *, *, #11653, .F. ) ;
#6355 = CARTESIAN_POINT ( 'NONE',  ( 2.718131847775120402, 5.344160105509049963, -24.78765742476133482 ) ) ;
#6356 = DIRECTION ( 'NONE',  ( 0.000000000000000000, 0.000000000000000000, 1.000000000000000000 ) ) ;
#6357 = CARTESIAN_POINT ( 'NONE',  ( -5.574407415329146964, 1.493657965219562067, -13.50000000000000533 ) ) ;
#6358 = CARTESIAN_POINT ( 'NONE',  ( -1.899999999999999023, 0.000000000000000000, 0.000000000000000000 ) ) ;
#6359 = CARTESIAN_POINT ( 'NONE',  ( -4.781284448697179279, 1.016293382781477961, -10.84374999795161543 ) ) ;
#6360 = ORIENTED_EDGE ( 'NONE', *, *, #6250, .F. ) ;
#6361 = CARTESIAN_POINT ( 'NONE',  ( 6.000000000000005329, 0.000000000000000000, 0.000000000000000000 ) ) ;
#6362 = CARTESIAN_POINT ( 'NONE',  ( 9.343749997951615427, -3.499494075959840966, 3.499494075959792116 ) ) ;
#6363 = ORIENTED_EDGE ( 'NONE', *, *, #17641, .F. ) ;
#6364 = CARTESIAN_POINT ( 'NONE',  ( 0.006974674093432157128, -2.249040938978327908, -24.42374957165208116 ) ) ;
#6365 = ADVANCED_FACE ( 'NONE', ( #7048 ), #13182, .F. ) ;
#6366 = EDGE_CURVE ( 'NONE', #14247, #18527, #7554, .T. ) ;
#6367 = CARTESIAN_POINT ( 'NONE',  ( -9.671566133830877376, 15.77352024078954429, -32.00000000000000000 ) ) ;
#6368 = AXIS2_PLACEMENT_3D ( 'NONE', #9337, #15539, #1826 ) ;
#6369 = VECTOR ( 'NONE', #10441, 1000.000000000000000 ) ;
#6370 = CYLINDRICAL_SURFACE ( 'NONE', #8049, 1.000000000000002665 ) ;
#6371 = FACE_OUTER_BOUND ( 'NONE', #534, .T. ) ;
#6372 = CARTESIAN_POINT ( 'NONE',  ( 0.02436607992776108206, -24.15498966839966855, 5.391175441198523544 ) ) ;
#6373 = ORIENTED_EDGE ( 'NONE', *, *, #11743, .T. ) ;
#6374 = CARTESIAN_POINT ( 'NONE',  ( 9.500000000000003553, 5.142044285764749922, -2.620002426024544473 ) ) ;
#6375 = DIRECTION ( 'NONE',  ( 1.000000000000000000, 0.000000000000000000, 0.000000000000000000 ) ) ;
#6376 = ORIENTED_EDGE ( 'NONE', *, *, #14904, .T. ) ;
#6377 = CARTESIAN_POINT ( 'NONE',  ( 2.789999999999999147, 0.000000000000000000, 0.000000000000000000 ) ) ;
#6378 = LINE ( 'NONE', #12507, #2643 ) ;
#6379 = CARTESIAN_POINT ( 'NONE',  ( 12.00000000000000533, 1.185096637661215757, 5.575441324182695446 ) ) ;
#6380 = FACE_OUTER_BOUND ( 'NONE', #9822, .T. ) ;
#6381 = EDGE_LOOP ( 'NONE', ( #16444, #13913, #17642, #16904 ) ) ;
#6382 = DIRECTION ( 'NONE',  ( 1.000000000000000000, 0.000000000000000000, 0.000000000000000000 ) ) ;
#6383 = ADVANCED_FACE ( 'NONE', ( #5276 ), #9803, .T. ) ;
#6384 = VECTOR ( 'NONE', #8792, 1000.000000000000000 ) ;
#6385 = DIRECTION ( 'NONE',  ( 0.000000000000000000, 0.000000000000000000, 1.000000000000000000 ) ) ;
#6386 = EDGE_CURVE ( 'NONE', #22, #4121, #970, .T. ) ;
#6387 = VECTOR ( 'NONE', #5383, 1000.000000000000000 ) ;
#6388 = VERTEX_POINT ( 'NONE', #9898 ) ;
#6389 = CARTESIAN_POINT ( 'NONE',  ( 9.000000000000005329, -0.5958122406255588199, -5.668774803599165857 ) ) ;
#6390 = CYLINDRICAL_SURFACE ( 'NONE', #12980, 28.06981291497571362 ) ;
#6391 = ORIENTED_EDGE ( 'NONE', *, *, #7081, .F. ) ;
#6392 = DIRECTION ( 'NONE',  ( -1.000000000000000000, -0.000000000000000000, -0.000000000000000000 ) ) ;
#6393 = CARTESIAN_POINT ( 'NONE',  ( 5.510910596163084625E-16, 18.00000000000000355, -32.00000000000000000 ) ) ;
#6394 = ORIENTED_EDGE ( 'NONE', *, *, #15285, .F. ) ;
#6395 = CIRCLE ( 'NONE', #16006, 12.00000000000000178 ) ;
#6396 = FACE_OUTER_BOUND ( 'NONE', #19047, .T. ) ;
#6397 = CARTESIAN_POINT ( 'NONE',  ( -10.00000000000000000, 0.000000000000000000, 0.000000000000000000 ) ) ;
#6398 = EDGE_CURVE ( 'NONE', #6283, #8351, #17164, .T. ) ;
#6399 = EDGE_LOOP ( 'NONE', ( #15961, #6512 ) ) ;
#6400 = DIRECTION ( 'NONE',  ( 1.000000000000000000, 0.000000000000000000, 0.000000000000000000 ) ) ;
#6401 = ORIENTED_EDGE ( 'NONE', *, *, #10994, .T. ) ;
#6402 = DIRECTION ( 'NONE',  ( 0.000000000000000000, 0.000000000000000000, -1.000000000000000000 ) ) ;
#6403 = VERTEX_POINT ( 'NONE', #5464 ) ;
#6404 = DIRECTION ( 'NONE',  ( -0.000000000000000000, -0.000000000000000000, 1.000000000000000000 ) ) ;
#6405 = CYLINDRICAL_SURFACE ( 'NONE', #13646, 1.000000000000002665 ) ;
#6406 = DIRECTION ( 'NONE',  ( -0.000000000000000000, -0.000000000000000000, 1.000000000000000000 ) ) ;
#6407 = EDGE_CURVE ( 'NONE', #11503, #8180, #11578, .T. ) ;
#6408 = CARTESIAN_POINT ( 'NONE',  ( 4.780397808154266848, 1.280903732194421218, -9.343749997951615427 ) ) ;
#6409 = EDGE_LOOP ( 'NONE', ( #75, #7566, #946, #14750, #3446, #14521 ) ) ;
#6410 = CARTESIAN_POINT ( 'NONE',  ( 0.1587402281127123227, 22.38003579136345067, 12.81821841996081801 ) ) ;
#6411 = CARTESIAN_POINT ( 'NONE',  ( -0.8944271909999155223, 0.000000000000000000, 0.000000000000000000 ) ) ;
#6412 = AXIS2_PLACEMENT_3D ( 'NONE', #16652, #10457, #2838 ) ;
#6413 = CIRCLE ( 'NONE', #1051, 8.000000000000000000 ) ;
#6414 = CIRCLE ( 'NONE', #7368, 4.000000000000000000 ) ;
#6415 = ORIENTED_EDGE ( 'NONE', *, *, #4751, .T. ) ;
#6416 = CARTESIAN_POINT ( 'NONE',  ( 2.255998204157473097, -17.85806462366060288, -32.00000000000000000 ) ) ;
#6417 = FACE_OUTER_BOUND ( 'NONE', #18974, .T. ) ;
#6418 = EDGE_LOOP ( 'NONE', ( #19219, #18555, #8003, #2047 ) ) ;
#6419 = LINE ( 'NONE', #15457, #18826 ) ;
#6420 = DIRECTION ( 'NONE',  ( -0.000000000000000000, -0.000000000000000000, 1.000000000000000000 ) ) ;
#6421 = ORIENTED_EDGE ( 'NONE', *, *, #18205, .T. ) ;
#6422 = CARTESIAN_POINT ( 'NONE',  ( 2.999999999999998224, 0.000000000000000000, 0.000000000000000000 ) ) ;
#6423 = EDGE_CURVE ( 'NONE', #18627, #17326, #17468, .T. ) ;
#6424 = CIRCLE ( 'NONE', #14113, 2.524999999999996358 ) ;
#6425 = ORIENTED_EDGE ( 'NONE', *, *, #5365, .F. ) ;
#6426 = PRODUCT_CONTEXT ( 'NONE', #9843, 'mechanical' ) ;
#6427 = CIRCLE ( 'NONE', #11560, 8.073750000000021743 ) ;
#6428 = CARTESIAN_POINT ( 'NONE',  ( -11.32184790671638730, 13.12143529358541549, 35.00000000000000000 ) ) ;
#6429 = CARTESIAN_POINT ( 'NONE',  ( 0.000000000000000000, 0.000000000000000000, -30.00000000000000355 ) ) ;
#6430 = VECTOR ( 'NONE', #2899, 1000.000000000000000 ) ;
#6431 = ORIENTED_EDGE ( 'NONE', *, *, #7510, .F. ) ;
#6432 = ORIENTED_EDGE ( 'NONE', *, *, #5813, .T. ) ;
#6433 = FACE_OUTER_BOUND ( 'NONE', #13692, .T. ) ;
#6434 = CARTESIAN_POINT ( 'NONE',  ( -9.580134541264520465, -14.56230589874905235, 35.00000000000000000 ) ) ;
#6435 = EDGE_CURVE ( 'NONE', #15675, #1756, #5251, .T. ) ;
#6436 = ORIENTED_EDGE ( 'NONE', *, *, #14703, .T. ) ;
#6437 = AXIS2_PLACEMENT_3D ( 'NONE', #12496, #3489, #13900 ) ;
#6438 = VERTEX_POINT ( 'NONE', #10480 ) ;
#6439 = VECTOR ( 'NONE', #3480, 1000.000000000000000 ) ;
#6440 = CIRCLE ( 'NONE', #7396, 7.500000000000000000 ) ;
#6441 = CARTESIAN_POINT ( 'NONE',  ( -0.5958122406256771697, -5.668774803599153422, -8.000000000000005329 ) ) ;
#6442 = CIRCLE ( 'NONE', #17325, 0.9999999999999974465 ) ;
#6443 = CARTESIAN_POINT ( 'NONE',  ( 0.000000000000000000, 0.000000000000000000, 6.000000000000000000 ) ) ;
#6444 = FACE_BOUND ( 'NONE', #13532, .T. ) ;
#6445 = EDGE_LOOP ( 'NONE', ( #4164, #10036, #7733, #3220 ) ) ;
#6446 = LINE ( 'NONE', #14069, #7555 ) ;
#6447 = ORIENTED_EDGE ( 'NONE', *, *, #9297, .T. ) ;
#6448 = ORIENTED_EDGE ( 'NONE', *, *, #12944, .F. ) ;
#6449 = CARTESIAN_POINT ( 'NONE',  ( 2.601776096565022289, -12.84621645676828372, -22.54313264455027976 ) ) ;
#6450 = AXIS2_PLACEMENT_3D ( 'NONE', #10389, #19768, #4375 ) ;
#6451 = CARTESIAN_POINT ( 'NONE',  ( -4.484949146646406426, -3.631840208645764179, -11.81249999590322552 ) ) ;
#6452 = ADVANCED_FACE ( 'NONE', ( #10383 ), #5860, .F. ) ;
#6453 = DIRECTION ( 'NONE',  ( 1.000000000000000000, 0.000000000000000000, 0.000000000000000000 ) ) ;
#6454 = TOROIDAL_SURFACE ( 'NONE', #12247, 24.12539914357697413, 8.000000000000000000 ) ;
#6455 = CARTESIAN_POINT ( 'NONE',  ( -2.620002426024544473, 5.142044285764749922, -9.500000000000003553 ) ) ;
#6456 = ORIENTED_EDGE ( 'NONE', *, *, #5135, .T. ) ;
#6457 = CARTESIAN_POINT ( 'NONE',  ( 2.604434261026090880, -25.39738473784997552, -5.253342437939998888 ) ) ;
#6458 = VECTOR ( 'NONE', #2045, 1000.000000000000000 ) ;
#6459 = DIRECTION ( 'NONE',  ( 1.000000000000000000, 0.000000000000000000, 0.000000000000000000 ) ) ;
#6460 = ORIENTED_EDGE ( 'NONE', *, *, #14395, .T. ) ;
#6461 = CARTESIAN_POINT ( 'NONE',  ( 14.00000000000000533, 5.668774803599165857, -0.5958122406255597081 ) ) ;
#6462 = DIRECTION ( 'NONE',  ( 0.000000000000000000, 0.000000000000000000, -1.000000000000000000 ) ) ;
#6463 = AXIS2_PLACEMENT_3D ( 'NONE', #18064, #2541, #14960 ) ;
#6464 = LINE ( 'NONE', #593, #3256 ) ;
#6465 = DIRECTION ( 'NONE',  ( -1.000000000000000000, 0.000000000000000000, 0.000000000000000000 ) ) ;
#6466 = ADVANCED_FACE ( 'NONE', ( #13464 ), #5151, .T. ) ;
#6467 = CARTESIAN_POINT ( 'NONE',  ( 4.648860486681943627, -1.510506337161893864, -7.468749997951615427 ) ) ;
#6468 = EDGE_LOOP ( 'NONE', ( #17204, #1647, #11480, #15460 ) ) ;
#6469 = VECTOR ( 'NONE', #9453, 1000.000000000000000 ) ;
#6470 = FACE_OUTER_BOUND ( 'NONE', #17872, .T. ) ;
#6471 = SHAPE_REPRESENTATION_RELATIONSHIP ( 'NONE' , 'NONE' ,  #6040, #9489 ) ;
#6472 = DIRECTION ( 'NONE',  ( 1.000000000000000000, 0.000000000000000000, 0.000000000000000000 ) ) ;
#6473 = CIRCLE ( 'NONE', #9376, 28.06981291497571007 ) ;
#6474 = DIRECTION ( 'NONE',  ( 0.000000000000000000, 0.000000000000000000, 1.000000000000000000 ) ) ;
#6475 = ORIENTED_EDGE ( 'NONE', *, *, #1325, .T. ) ;
#6476 = CARTESIAN_POINT ( 'NONE',  ( 15.28688694438835505, -7.664027248171309203, 32.00000000000000000 ) ) ;
#6477 = EDGE_CURVE ( 'NONE', #13404, #7114, #471, .T. ) ;
#6478 = FACE_OUTER_BOUND ( 'NONE', #14255, .T. ) ;
#6479 = CARTESIAN_POINT ( 'NONE',  ( 11.46874999795161543, 2.444050593749990785, 4.233219804643887585 ) ) ;
#6480 = CARTESIAN_POINT ( 'NONE',  ( 0.000000000000000000, 0.000000000000000000, -29.00000000000000000 ) ) ;
#6481 = DIRECTION ( 'NONE',  ( -1.000000000000000000, 0.000000000000000000, -0.000000000000000000 ) ) ;
#6482 = ORIENTED_EDGE ( 'NONE', *, *, #17607, .F. ) ;
#6483 = EDGE_CURVE ( 'NONE', #12253, #10545, #11975, .T. ) ;
#6484 = CARTESIAN_POINT ( 'NONE',  ( -4.476417968967385974, 17.43449690031536292, 35.00000000000000000 ) ) ;
#6485 =( GEOMETRIC_REPRESENTATION_CONTEXT ( 3 ) GLOBAL_UNCERTAINTY_ASSIGNED_CONTEXT ( ( #14991 ) ) GLOBAL_UNIT_ASSIGNED_CONTEXT ( ( #10803, #10708, #15312 ) ) REPRESENTATION_CONTEXT ( 'NONE', 'WORKASPACE' ) );
#6486 = CYLINDRICAL_SURFACE ( 'NONE', #10484, 2.524999999999995914 ) ;
#6487 = ORIENTED_EDGE ( 'NONE', *, *, #6277, .F. ) ;
#6488 = CARTESIAN_POINT ( 'NONE',  ( 13.34374999795161365, -4.409619785863891472, -2.246813503491864150 ) ) ;
#6489 = B_SPLINE_CURVE_WITH_KNOTS ( 'NONE', 3,
 ( #5366, #15254, #9146, #12250 ),
 .UNSPECIFIED., .F., .F.,
 ( 4, 4 ),
 ( 0.005258214619651955385, 0.005948481662034169927 ),
 .UNSPECIFIED. ) ;
#6490 = CARTESIAN_POINT ( 'NONE',  ( -4.500000000000000000, 0.000000000000000000, -33.00000000000000000 ) ) ;
#6491 = ORIENTED_EDGE ( 'NONE', *, *, #13098, .F. ) ;
#6492 = B_SPLINE_CURVE_WITH_KNOTS ( 'NONE', 3,
 ( #17362, #657, #9566, #8352, #14564, #3649 ),
 .UNSPECIFIED., .F., .F.,
 ( 4, 2, 4 ),
 ( 2.380731676487269046E-07, 0.002318718087522257665, 0.004637198101876866679 ),
 .UNSPECIFIED. ) ;
#6493 = CIRCLE ( 'NONE', #13855, 8.073750000000021743 ) ;
#6494 = ADVANCED_FACE ( 'NONE', ( #7245 ), #19469, .F. ) ;
#6495 = LINE ( 'NONE', #15526, #8363 ) ;
#6496 = CARTESIAN_POINT ( 'NONE',  ( 8.312499995903225525, 1.761396867937200517, -5.421022142882375938 ) ) ;
#6497 = ORIENTED_EDGE ( 'NONE', *, *, #16183, .F. ) ;
#6498 = FACE_OUTER_BOUND ( 'NONE', #12928, .T. ) ;
#6499 = ADVANCED_FACE ( 'NONE', ( #11871 ), #17304, .T. ) ;
#6500 = CARTESIAN_POINT ( 'NONE',  ( 1.510506337161861223, 4.648860486681953397, -12.46874999795161543 ) ) ;
#6501 = ORIENTED_EDGE ( 'NONE', *, *, #13356, .F. ) ;
#6502 = DIRECTION ( 'NONE',  ( 0.000000000000000000, 0.000000000000000000, -1.000000000000000000 ) ) ;
#6503 = VERTEX_POINT ( 'NONE', #1269 ) ;
#6504 =( BOUNDED_CURVE ( )  B_SPLINE_CURVE ( 2, ( #7764, #13877, #1569, #6252, #12378, #555, #12751, #5132, #11246, #10245, #2717, #8834, #14838, #4131, #5618 ),
 .UNSPECIFIED., .F., .F. ) 
 B_SPLINE_CURVE_WITH_KNOTS ( ( 3, 2, 2, 2, 2, 2, 2, 3 ),
 ( 0.000000000000000000, 0.05000000000000000278, 0.1000000000000000056, 0.1499999999999999944, 0.2000000000000000111, 0.2500000000000000000, 0.2999999999999999889, 0.3078686208676164604 ),
 .UNSPECIFIED. ) 
 CURVE ( )  GEOMETRIC_REPRESENTATION_ITEM ( )  RATIONAL_B_SPLINE_CURVE ( ( 1.000000000000000000, 0.9876883405951377704, 1.000000000000000000, 0.9876883405951377704, 1.000000000000000000, 0.9876883405951377704, 1.000000000000000000, 0.9876883405951377704, 1.000000000000000000, 0.9876883405951377704, 1.000000000000000000, 0.9876883405951377704, 1.000000000000000000, 0.9980624843978382899, 0.9967347918236166837 ) ) 
 REPRESENTATION_ITEM ( '' )  );
#6505 = CARTESIAN_POINT ( 'NONE',  ( 2.789999999999999147, -22.25075486061744812, 9.324097380959361914 ) ) ;
#6506 = VERTEX_POINT ( 'NONE', #19338 ) ;
#6507 = CARTESIAN_POINT ( 'NONE',  ( 0.000000000000000000, 0.000000000000000000, -18.00000000000000355 ) ) ;
#6508 = AXIS2_PLACEMENT_3D ( 'NONE', #594, #886, #793 ) ;
#6509 = CARTESIAN_POINT ( 'NONE',  ( 2.765633920072235963, 24.63872515616082737, 2.336989772644355146 ) ) ;
#6510 = CARTESIAN_POINT ( 'NONE',  ( -30.00000000000000000, -1.925929944387235853E-31, 0.000000000000000000 ) ) ;
#6511 = CARTESIAN_POINT ( 'NONE',  ( 4.233219804643871598, -2.444050593750019651, -11.46874999795161543 ) ) ;
#6512 = ORIENTED_EDGE ( 'NONE', *, *, #5175, .F. ) ;
#6513 = DIRECTION ( 'NONE',  ( 0.000000000000000000, 0.000000000000000000, 1.000000000000000000 ) ) ;
#6514 = CARTESIAN_POINT ( 'NONE',  ( 2.789999999999999147, 0.000000000000000000, 0.000000000000000000 ) ) ;
#6515 = AXIS2_PLACEMENT_3D ( 'NONE', #18473, #18669, #4967 ) ;
#6516 = ORIENTED_EDGE ( 'NONE', *, *, #504, .T. ) ;
#6517 = EDGE_CURVE ( 'NONE', #8963, #12765, #2906, .T. ) ;
#6518 = DIRECTION ( 'NONE',  ( 0.000000000000000000, 0.000000000000000000, 1.000000000000000000 ) ) ;
#6519 = AXIS2_PLACEMENT_3D ( 'NONE', #3420, #526, #17324 ) ;
#6520 = CARTESIAN_POINT ( 'NONE',  ( -2.299999999999996270, 0.000000000000000000, 0.000000000000000000 ) ) ;
#6521 = CYLINDRICAL_SURFACE ( 'NONE', #753, 1.000000000000000888 ) ;
#6522 = ORIENTED_EDGE ( 'NONE', *, *, #7803, .F. ) ;
#6523 = CARTESIAN_POINT ( 'NONE',  ( 6.500000000000005329, -5.387740456496247887, 2.068159791354145849 ) ) ;
#6524 = CARTESIAN_POINT ( 'NONE',  ( 13.31249999590322730, 4.235925505221192822, -3.814044456245444081 ) ) ;
#6525 = ORIENTED_EDGE ( 'NONE', *, *, #7556, .T. ) ;
#6526 = FACE_OUTER_BOUND ( 'NONE', #16957, .T. ) ;
#6527 = CIRCLE ( 'NONE', #12623, 28.06981291497571007 ) ;
#6528 = ORIENTED_EDGE ( 'NONE', *, *, #15670, .F. ) ;
#6529 = B_SPLINE_CURVE_WITH_KNOTS ( 'NONE', 3,
 ( #12636, #18630, #3523, #3819, #14632, #18926 ),
 .UNSPECIFIED., .F., .F.,
 ( 4, 2, 4 ),
 ( 2.132675795051084930E-07, 0.001878604073277006722, 0.003756994878974508241 ),
 .UNSPECIFIED. ) ;
#6530 = APPLICATION_PROTOCOL_DEFINITION ( 'draft international standard', 'automotive_design', 1998, #10473 ) ;
#6531 = CARTESIAN_POINT ( 'NONE',  ( 2.000000000000001776, 0.000000000000000000, 0.000000000000000000 ) ) ;
#6532 = FILL_AREA_STYLE ('',( #457 ) ) ;
#6533 = ORIENTED_EDGE ( 'NONE', *, *, #8183, .F. ) ;
#6534 = ORIENTED_EDGE ( 'NONE', *, *, #3700, .T. ) ;
#6535 = CARTESIAN_POINT ( 'NONE',  ( 10.58013454126452046, -14.56230589874905412, -32.00000000000000000 ) ) ;
#6536 = CARTESIAN_POINT ( 'NONE',  ( 11.46874999795161543, -2.444050593750019651, 4.233219804643871598 ) ) ;
#6537 = EDGE_LOOP ( 'NONE', ( #10450, #1639, #10173, #10534 ) ) ;
#6538 =( NAMED_UNIT ( * ) SI_UNIT ( $, .STERADIAN. ) SOLID_ANGLE_UNIT ( ) );
#6539 = EDGE_CURVE ( 'NONE', #9343, #16572, #19052, .T. ) ;
#6540 = ORIENTED_EDGE ( 'NONE', *, *, #1951, .F. ) ;
#6541 = AXIS2_PLACEMENT_3D ( 'NONE', #6621, #8629, #8340 ) ;
#6542 = CARTESIAN_POINT ( 'NONE',  ( -41.99999999999999289, -5.000000000000001776, 5.000000000000000000 ) ) ;
#6543 = ADVANCED_FACE ( 'NONE', ( #19438 ), #5341, .F. ) ;
#6544 = DIRECTION ( 'NONE',  ( 0.000000000000000000, 0.000000000000000000, 1.000000000000000000 ) ) ;
#6545 = CARTESIAN_POINT ( 'NONE',  ( 2.601776121706764311, -17.47009390565504816, 19.18368891937484477 ) ) ;
#6546 = VERTEX_POINT ( 'NONE', #8642 ) ;
#6547 = CARTESIAN_POINT ( 'NONE',  ( 0.006931054464084583991, -2.248820353273142558, 24.42321038836782776 ) ) ;
#6548 = CARTESIAN_POINT ( 'NONE',  ( 2.000000000000000000, -2.000000000000002665, 37.99999999999999289 ) ) ;
#6549 = ORIENTED_EDGE ( 'NONE', *, *, #3458, .F. ) ;
#6550 = VERTEX_POINT ( 'NONE', #17748 ) ;
#6551 = CARTESIAN_POINT ( 'NONE',  ( -3.114526743279308896, -3.846120219227901149, -6.968749997951614539 ) ) ;
#6552 = AXIS2_PLACEMENT_3D ( 'NONE', #2630, #8742, #11841 ) ;
#6553 = ADVANCED_FACE ( 'NONE', ( #13250 ), #11744, .T. ) ;
#6554 = CIRCLE ( 'NONE', #4337, 28.06981291497571007 ) ;
#6555 = DIRECTION ( 'NONE',  ( 1.000000000000000000, 0.000000000000000000, 0.000000000000000000 ) ) ;
#6556 = CARTESIAN_POINT ( 'NONE',  ( -3.954556930911862000, 2.873153789725825469, -8.468749997951615427 ) ) ;
#6557 = EDGE_LOOP ( 'NONE', ( #3850, #9763, #13981, #16885 ) ) ;
#6558 = DIRECTION ( 'NONE',  ( 1.000000000000000000, 0.000000000000000000, 0.000000000000000000 ) ) ;
#6559 = DIRECTION ( 'NONE',  ( -1.000000000000000000, 0.000000000000000000, 0.000000000000000000 ) ) ;
#6560 = B_SPLINE_CURVE_WITH_KNOTS ( 'NONE', 3,
 ( #14089, #495, #6568, #4792, #13901, #14294 ),
 .UNSPECIFIED., .F., .F.,
 ( 4, 2, 4 ),
 ( 4.462636732176736601E-07, 0.001879885066974997356, 0.003759323870276777037 ),
 .UNSPECIFIED. ) ;
#6561 = ORIENTED_EDGE ( 'NONE', *, *, #838, .T. ) ;
#6562 = LINE ( 'NONE', #8385, #2398 ) ;
#6563 = DIRECTION ( 'NONE',  ( -1.000000000000000000, -0.000000000000000000, -0.000000000000000000 ) ) ;
#6564 = AXIS2_PLACEMENT_3D ( 'NONE', #17715, #2111, #19207 ) ;
#6565 = EDGE_CURVE ( 'NONE', #15969, #15613, #2595, .T. ) ;
#6566 = CIRCLE ( 'NONE', #7529, 1.000000000000002665 ) ;
#6567 = CYLINDRICAL_SURFACE ( 'NONE', #16693, 13.19999999999999929 ) ;
#6568 = CARTESIAN_POINT ( 'NONE',  ( 0.5321745326902584949, 3.467596033028283564, 26.83036154824995023 ) ) ;
#6569 = CARTESIAN_POINT ( 'NONE',  ( 7.843749997951614539, 4.781284448697194378, -1.016293382781411569 ) ) ;
#6570 = ORIENTED_EDGE ( 'NONE', *, *, #4518, .T. ) ;
#6571 = PLANE ( 'NONE',  #1174 ) ;
#6572 = DIRECTION ( 'NONE',  ( 0.6363829547955638377, 7.793443486223220387E-17, -0.7713732785400770897 ) ) ;
#6573 = CARTESIAN_POINT ( 'NONE',  ( 3.143139765844622957, 4.840010801796482909, -10.81249999590322375 ) ) ;
#6574 = ORIENTED_EDGE ( 'NONE', *, *, #3722, .T. ) ;
#6575 = DIRECTION ( 'NONE',  ( 0.000000000000000000, 0.000000000000000000, 1.000000000000000000 ) ) ;
#6576 = PRODUCT_DEFINITION_CONTEXT ( 'detailed design', #7767, 'design' ) ;
#6577 = CARTESIAN_POINT ( 'NONE',  ( 6.500000000000005329, 5.387740456496233676, -2.068159791354183596 ) ) ;
#6578 = DIRECTION ( 'NONE',  ( 0.000000000000000000, 0.000000000000000000, 1.000000000000000000 ) ) ;
#6579 = CARTESIAN_POINT ( 'NONE',  ( 0.5109457054261454800, -4.861323657744410554, -14.46874999795161720 ) ) ;
#6580 = ORIENTED_EDGE ( 'NONE', *, *, #11742, .F. ) ;
#6581 = CARTESIAN_POINT ( 'NONE',  ( 5.574407415329157622, -1.493657965219523209, -14.81249999590322375 ) ) ;
#6582 = VECTOR ( 'NONE', #18404, 1000.000000000000000 ) ;
#6583 = DIRECTION ( 'NONE',  ( 1.000000000000000000, 0.000000000000000000, 0.000000000000000000 ) ) ;
#6584 = CIRCLE ( 'NONE', #17785, 0.1999999999999996503 ) ;
#6585 = ORIENTED_EDGE ( 'NONE', *, *, #15930, .T. ) ;
#6586 = CARTESIAN_POINT ( 'NONE',  ( 8.812499995903225525, -2.620002426024580000, 5.142044285764733935 ) ) ;
#6587 = ADVANCED_FACE ( 'NONE', ( #10253 ), #852, .F. ) ;
#6588 = DIRECTION ( 'NONE',  ( -1.000000000000000000, 0.000000000000000000, 0.000000000000000000 ) ) ;
#6589 = ORIENTED_EDGE ( 'NONE', *, *, #7061, .T. ) ;
#6590 = EDGE_CURVE ( 'NONE', #1462, #5861, #3945, .T. ) ;
#6591 = CARTESIAN_POINT ( 'NONE',  ( 0.000000000000000000, 0.000000000000000000, 0.000000000000000000 ) ) ;
#6592 = CARTESIAN_POINT ( 'NONE',  ( 12.99999999999969980, 5.254364458093119694, 1.428050399360184963 ) ) ;
#6593 = EDGE_CURVE ( 'NONE', #11735, #1617, #14756, .T. ) ;
#6594 = ORIENTED_EDGE ( 'NONE', *, *, #4568, .F. ) ;
#6595 = VECTOR ( 'NONE', #2972, 1000.000000000000000 ) ;
#6596 = CYLINDRICAL_SURFACE ( 'NONE', #15537, 1.000000000000003553 ) ;
#6597 = CARTESIAN_POINT ( 'NONE',  ( 2.783025325906568259, 24.42374957165205629, 2.249040938978581927 ) ) ;
#6598 = CARTESIAN_POINT ( 'NONE',  ( 2.873153789725825025, 3.954556930911862000, -13.46874999795161543 ) ) ;
#6599 = AXIS2_PLACEMENT_3D ( 'NONE', #7668, #19585, #16894 ) ;
#6600 = ORIENTED_EDGE ( 'NONE', *, *, #16003, .F. ) ;
#6601 = LINE ( 'NONE', #15631, #6066 ) ;
#6602 = ORIENTED_EDGE ( 'NONE', *, *, #6847, .F. ) ;
#6603 = PLANE ( 'NONE',  #9193 ) ;
#6604 = B_SPLINE_CURVE_WITH_KNOTS ( 'NONE', 3,
 ( #6167, #8984, #18192, #18287 ),
 .UNSPECIFIED., .F., .F.,
 ( 4, 4 ),
 ( 4.462636695653741059E-07, 0.0004963285629696456008 ),
 .UNSPECIFIED. ) ;
#6605 = EDGE_LOOP ( 'NONE', ( #245, #8350 ) ) ;
#6606 = FACE_OUTER_BOUND ( 'NONE', #4111, .T. ) ;
#6607 = FACE_OUTER_BOUND ( 'NONE', #3424, .T. ) ;
#6608 = CARTESIAN_POINT ( 'NONE',  ( 0.1855655959470679794, 19.17825124759777822, 17.45907811351462158 ) ) ;
#6609 = VERTEX_POINT ( 'NONE', #16059 ) ;
#6610 = CARTESIAN_POINT ( 'NONE',  ( 2.500000000000002220, 0.000000000000000000, -8.073750000000021743 ) ) ;
#6611 = CARTESIAN_POINT ( 'NONE',  ( -36.00000000000000000, 4.400000000000000355, 0.000000000000000000 ) ) ;
#6612 = VECTOR ( 'NONE', #15315, 1000.000000000000000 ) ;
#6613 = ORIENTED_EDGE ( 'NONE', *, *, #17036, .F. ) ;
#6614 = AXIS2_PLACEMENT_3D ( 'NONE', #5191, #16186, #8568 ) ;
#6615 = CARTESIAN_POINT ( 'NONE',  ( 3.954556930911861112, 2.873153789725825913, -14.84374999795161543 ) ) ;
#6616 = EDGE_CURVE ( 'NONE', #12779, #12621, #16344, .T. ) ;
#6617 = DIRECTION ( 'NONE',  ( -1.000000000000000000, 0.000000000000000000, 0.000000000000000000 ) ) ;
#6618 = CARTESIAN_POINT ( 'NONE',  ( -4.465502636338010589, 1.988169868018623720, -14.46874999795161720 ) ) ;
#6619 = EDGE_CURVE ( 'NONE', #14047, #18333, #52, .T. ) ;
#6620 = ORIENTED_EDGE ( 'NONE', *, *, #4814, .F. ) ;
#6621 = CARTESIAN_POINT ( 'NONE',  ( -2.299999999999996270, 0.000000000000000000, 0.000000000000000000 ) ) ;
#6622 = CARTESIAN_POINT ( 'NONE',  ( 9.812499995903223748, -1.493657965219446382, -5.574407415329178939 ) ) ;
#6623 = DIRECTION ( 'NONE',  ( 1.000000000000000000, 0.000000000000000000, 0.000000000000000000 ) ) ;
#6624 = ORIENTED_EDGE ( 'NONE', *, *, #4736, .F. ) ;
#6625 = CARTESIAN_POINT ( 'NONE',  ( -5.700000000000001066, 1.090170143537592985E-15, -10.64522241986045259 ) ) ;
#6626 = AXIS2_PLACEMENT_3D ( 'NONE', #16592, #10588, #4285 ) ;
#6627 = ORIENTED_EDGE ( 'NONE', *, *, #3744, .T. ) ;
#6628 = CARTESIAN_POINT ( 'NONE',  ( 1.255998204157470211, -17.85806462366060288, -35.00000000000000000 ) ) ;
#6629 = AXIS2_PLACEMENT_3D ( 'NONE', #17630, #11435, #4020 ) ;
#6630 = CARTESIAN_POINT ( 'NONE',  ( 9.843749997951615427, 4.465502636338023912, 1.988169868018593300 ) ) ;
#6631 = EDGE_CURVE ( 'NONE', #3616, #12101, #13054, .T. ) ;
#6632 = VERTEX_POINT ( 'NONE', #8740 ) ;
#6633 = VERTEX_POINT ( 'NONE', #14847 ) ;
#6634 = FACE_OUTER_BOUND ( 'NONE', #14288, .T. ) ;
#6635 = CARTESIAN_POINT ( 'NONE',  ( 12.46874999795161543, -3.632567103900546712, 3.270778111535314281 ) ) ;
#6636 = ORIENTED_EDGE ( 'NONE', *, *, #4836, .F. ) ;
#6637 = EDGE_CURVE ( 'NONE', #17341, #13082, #6743, .T. ) ;
#6638 = ADVANCED_FACE ( 'NONE', ( #17947 ), #4239, .F. ) ;
#6639 = CARTESIAN_POINT ( 'NONE',  ( 2.765633920072235963, 22.71065055754452544, 9.836394144775786330 ) ) ;
#6640 = PRODUCT_DEFINITION_SHAPE ( 'NONE', 'NONE',  #16784 ) ;
#6641 = VECTOR ( 'NONE', #13457, 1000.000000000000000 ) ;
#6642 = ORIENTED_EDGE ( 'NONE', *, *, #4278, .T. ) ;
#6643 = CARTESIAN_POINT ( 'NONE',  ( -3.143139765844656264, -4.840010801796461593, -9.500000000000005329 ) ) ;
#6644 = DIRECTION ( 'NONE',  ( 0.000000000000000000, 1.000000000000000000, 0.000000000000000000 ) ) ;
#6645 = FACE_BOUND ( 'NONE', #17012, .T. ) ;
#6646 = ORIENTED_EDGE ( 'NONE', *, *, #8070, .F. ) ;
#6647 = CARTESIAN_POINT ( 'NONE',  ( 1.039999999999997149, -24.89775460606822577, -12.96210679857813730 ) ) ;
#6648 =( LENGTH_UNIT ( ) NAMED_UNIT ( * ) SI_UNIT ( .MILLI., .METRE. ) );
#6649 = FACE_OUTER_BOUND ( 'NONE', #2624, .T. ) ;
#6650 = EDGE_CURVE ( 'NONE', #5753, #14722, #11547, .T. ) ;
#6651 = ORIENTED_EDGE ( 'NONE', *, *, #2579, .T. ) ;
#6652 = ORIENTED_EDGE ( 'NONE', *, *, #11909, .T. ) ;
#6653 = DIRECTION ( 'NONE',  ( 1.000000000000000000, 0.000000000000000000, 0.000000000000000000 ) ) ;
#6654 = VECTOR ( 'NONE', #2435, 1000.000000000000000 ) ;
#6655 = DIRECTION ( 'NONE',  ( 1.000000000000000000, 0.000000000000000000, 0.000000000000000000 ) ) ;
#6656 = EDGE_CURVE ( 'NONE', #9320, #13012, #945, .T. ) ;
#6657 = FACE_BOUND ( 'NONE', #112, .T. ) ;
#6658 = ADVANCED_FACE ( 'NONE', ( #5535 ), #11643, .T. ) ;
#6659 = VERTEX_POINT ( 'NONE', #7721 ) ;
#6660 = CARTESIAN_POINT ( 'NONE',  ( 11.34374999795161543, 1.773574444220790136, -4.620319390059805187 ) ) ;
#6661 = CARTESIAN_POINT ( 'NONE',  ( 9.843749997951615427, -3.954556930911881985, 2.873153789725797491 ) ) ;
#6662 = ORIENTED_EDGE ( 'NONE', *, *, #17607, .T. ) ;
#6663 = DIRECTION ( 'NONE',  ( 0.000000000000000000, 0.000000000000000000, 1.000000000000000000 ) ) ;
#6664 = CARTESIAN_POINT ( 'NONE',  ( 7.000000000000005329, 1.761396867937200517, -5.421022142882375938 ) ) ;
#6665 = VECTOR ( 'NONE', #10950, 1000.000000000000000 ) ;
#6666 = EDGE_CURVE ( 'NONE', #14571, #12630, #689, .T. ) ;
#6667 = DIRECTION ( 'NONE',  ( 0.000000000000000000, 0.000000000000000000, 1.000000000000000000 ) ) ;
#6668 = CARTESIAN_POINT ( 'NONE',  ( 2.790000000000000036, 18.34424029220134500, -15.96500990068104997 ) ) ;
#6669 = CARTESIAN_POINT ( 'NONE',  ( 9.671566133830877376, 15.77352024078954784, -32.00000000000000000 ) ) ;
#6670 = AXIS2_PLACEMENT_3D ( 'NONE', #10151, #11741, #6929 ) ;
#6671 = FACE_OUTER_BOUND ( 'NONE', #18548, .T. ) ;
#6672 = CARTESIAN_POINT ( 'NONE',  ( 13.86923836996420789, -11.47363181547641453, -32.00000000000000000 ) ) ;
#6673 =( LENGTH_UNIT ( ) NAMED_UNIT ( * ) SI_UNIT ( .MILLI., .METRE. ) );
#6674 = FILL_AREA_STYLE_COLOUR ( '', #336 ) ;
#6675 = ORIENTED_EDGE ( 'NONE', *, *, #7117, .F. ) ;
#6676 =( BOUNDED_SURFACE ( )  B_SPLINE_SURFACE ( 1, 2, ( 
 ( #19723, #7709, #5911, #6007, #1615, #19626, #4618, #10433, #12128, #18233, #9024, #13723, #12, #16933, #9126, #16535, #18133 ),
 ( #4511, #13825, #15231, #2811, #1524, #7399, #15428, #10528, #7609, #19518, #16625, #9324, #18327, #13523, #12029, #18422, #3210 ) ),
 .UNSPECIFIED., .F., .F., .T. ) 
 B_SPLINE_SURFACE_WITH_KNOTS ( ( 2, 2 ),
 ( 3, 2, 2, 2, 2, 2, 2, 2, 3 ),
 ( 0.000000000000000000, 1.000000000000000000 ),
 ( 0.000000000000000000, 0.05000000000000000278, 0.1000000000000000056, 0.1499999999999999944, 0.2000000000000000111, 0.2500000000000000000, 0.2999999999999999889, 0.3499999999999999778, 0.4000000000000000222 ),
 .UNSPECIFIED. ) 
 GEOMETRIC_REPRESENTATION_ITEM ( )  RATIONAL_B_SPLINE_SURFACE ( (
 ( 1.000000000000000000, 0.9876883405951377704, 1.000000000000000000, 0.9876883405951377704, 1.000000000000000000, 0.9876883405951377704, 1.000000000000000000, 0.9876883405951377704, 1.000000000000000000, 0.9876883405951377704, 1.000000000000000000, 0.9876883405951377704, 1.000000000000000000, 0.9876883405951377704, 1.000000000000000000, 0.9876883405951377704, 1.000000000000000000),
 ( 1.000000000000000000, 0.9876883405951377704, 1.000000000000000000, 0.9876883405951377704, 1.000000000000000000, 0.9876883405951377704, 1.000000000000000000, 0.9876883405951377704, 1.000000000000000000, 0.9876883405951377704, 1.000000000000000000, 0.9876883405951377704, 1.000000000000000000, 0.9876883405951377704, 1.000000000000000000, 0.9876883405951377704, 1.000000000000000000) ) ) 
 REPRESENTATION_ITEM ( '' )  SURFACE ( )  );
#6677 = CARTESIAN_POINT ( 'NONE',  ( 12.65441706489329299, 2.315350974882481871, 5.245024560144870840 ) ) ;
#6678 = LINE ( 'NONE', #9608, #16092 ) ;
#6679 = CARTESIAN_POINT ( 'NONE',  ( 3.846120219227923798, -3.114526743279282250, -12.34374999795161543 ) ) ;
#6680 = CARTESIAN_POINT ( 'NONE',  ( 12.46874999795161543, -3.632567103900546712, 3.270778111535314281 ) ) ;
#6681 = CARTESIAN_POINT ( 'NONE',  ( 9.843749997951615427, -4.465502636338009701, -1.988169868018624609 ) ) ;
#6682 = ORIENTED_EDGE ( 'NONE', *, *, #265, .T. ) ;
#6683 = DIRECTION ( 'NONE',  ( 0.000000000000000000, 0.000000000000000000, 1.000000000000000000 ) ) ;
#6684 = CARTESIAN_POINT ( 'NONE',  ( -4.888101187500000222, 0.000000000000000000, -6.843749997951615427 ) ) ;
#6685 = EDGE_CURVE ( 'NONE', #7112, #5154, #13791, .T. ) ;
#6686 = ORIENTED_EDGE ( 'NONE', *, *, #18735, .T. ) ;
#6687 = CARTESIAN_POINT ( 'NONE',  ( 10.81249999590322375, -5.142044285764769462, 2.620002426024508502 ) ) ;
#6688 = CARTESIAN_POINT ( 'NONE',  ( -7.937500000000000000, -4.582717761692662428, -6.527800000000000047 ) ) ;
#6689 = AXIS2_PLACEMENT_3D ( 'NONE', #11337, #17435, #3723 ) ;
#6690 = ORIENTED_EDGE ( 'NONE', *, *, #17404, .T. ) ;
#6691 = SURFACE_STYLE_FILL_AREA ( #18909 ) ;
#6692 = VECTOR ( 'NONE', #10635, 999.9999999999998863 ) ;
#6693 = PLANE ( 'NONE',  #9322 ) ;
#6694 = CARTESIAN_POINT ( 'NONE',  ( 11.81249999590322552, 5.700000000000000178, -0.9027913098498572264 ) ) ;
#6695 = VERTEX_POINT ( 'NONE', #2726 ) ;
#6696 = DIRECTION ( 'NONE',  ( -0.000000000000000000, -0.000000000000000000, 1.000000000000000000 ) ) ;
#6697 = DIRECTION ( 'NONE',  ( 1.000000000000000000, 6.419766481290786633E-33, -0.000000000000000000 ) ) ;
#6698 = CARTESIAN_POINT ( 'NONE',  ( 2.765633920072236851, 24.15498966839963302, 5.391175441198700291 ) ) ;
#6699 = ORIENTED_EDGE ( 'NONE', *, *, #3353, .T. ) ;
#6700 = ADVANCED_FACE ( 'NONE', ( #18145 ), #25, .T. ) ;
#6701 = CARTESIAN_POINT ( 'NONE',  ( 10.46874999795161720, -4.648860486681964055, 1.510506337161829027 ) ) ;
#6702 = ORIENTED_EDGE ( 'NONE', *, *, #19012, .T. ) ;
#6703 = FACE_OUTER_BOUND ( 'NONE', #2621, .T. ) ;
#6704 = ORIENTED_EDGE ( 'NONE', *, *, #7324, .T. ) ;
#6705 = AXIS2_PLACEMENT_3D ( 'NONE', #4352, #10460, #13552 ) ;
#6706 = PLANE ( 'NONE',  #6689 ) ;
#6707 = CARTESIAN_POINT ( 'NONE',  ( 3.476417968967386418, 17.43449690031536292, 32.00000000000000000 ) ) ;
#6708 = DIRECTION ( 'NONE',  ( 0.000000000000000000, -0.7315216790650492795, 0.6818181818181815457 ) ) ;
#6709 = CARTESIAN_POINT ( 'NONE',  ( 3.846120219227923798, -3.114526743279282250, -12.34374999795161543 ) ) ;
#6710 = ADVANCED_FACE ( 'NONE', ( #6119 ), #14426, .T. ) ;
#6711 = EDGE_CURVE ( 'NONE', #10395, #3050, #4051, .T. ) ;
#6712 = ORIENTED_EDGE ( 'NONE', *, *, #13235, .F. ) ;
#6713 = FACE_BOUND ( 'NONE', #12167, .T. ) ;
#6714 = DIRECTION ( 'NONE',  ( 0.000000000000000000, 0.000000000000000000, -1.000000000000000000 ) ) ;
#6715 = VERTEX_POINT ( 'NONE', #16848 ) ;
#6716 = DIRECTION ( 'NONE',  ( 0.000000000000000000, 0.000000000000000000, -1.000000000000000000 ) ) ;
#6717 = CYLINDRICAL_SURFACE ( 'NONE', #18566, 4.000000000000000000 ) ;
#6718 = CARTESIAN_POINT ( 'NONE',  ( 1.016293382781377819, -4.781284448697200595, -7.468749997951615427 ) ) ;
#6719 = VERTEX_POINT ( 'NONE', #15347 ) ;
#6720 = CARTESIAN_POINT ( 'NONE',  ( 0.7589665326895898012, 24.32849926382769468, -12.98167595240995986 ) ) ;
#6721 = CARTESIAN_POINT ( 'NONE',  ( 1.510506337161829027, -4.648860486681964055, -10.46874999795161720 ) ) ;
#6722 = DIRECTION ( 'NONE',  ( 0.000000000000000000, 0.000000000000000000, 1.000000000000000000 ) ) ;
#6723 = ORIENTED_EDGE ( 'NONE', *, *, #17251, .T. ) ;
#6724 = DIRECTION ( 'NONE',  ( 1.000000000000000000, 0.000000000000000000, 0.000000000000000000 ) ) ;
#6725 = ORIENTED_EDGE ( 'NONE', *, *, #3132, .T. ) ;
#6726 = CONTEXT_DEPENDENT_SHAPE_REPRESENTATION ( #18560, #10360 ) ;
#6727 = CARTESIAN_POINT ( 'NONE',  ( 11.84374999795161365, -2.444050593750019651, 4.233219804643871598 ) ) ;
#6728 = DIRECTION ( 'NONE',  ( 0.000000000000000000, 0.000000000000000000, 1.000000000000000000 ) ) ;
#6729 = ORIENTED_EDGE ( 'NONE', *, *, #2311, .T. ) ;
#6730 = ORIENTED_EDGE ( 'NONE', *, *, #8829, .F. ) ;
#6731 = CARTESIAN_POINT ( 'NONE',  ( 0.1570303611602991700, -22.37100459959352605, 12.81671916049007365 ) ) ;
#6732 = DIRECTION ( 'NONE',  ( 0.000000000000000000, 0.000000000000000000, 1.000000000000000000 ) ) ;
#6733 = CIRCLE ( 'NONE', #8670, 1.000000000000004441 ) ;
#6734 = DIRECTION ( 'NONE',  ( 0.8660254037844417052, -0.4999999999999947820, 0.000000000000000000 ) ) ;
#6735 = EDGE_LOOP ( 'NONE', ( #420, #1321, #4068, #6110 ) ) ;
#6736 = EDGE_CURVE ( 'NONE', #19457, #19757, #5777, .T. ) ;
#6737 = EDGE_CURVE ( 'NONE', #4959, #2904, #4510, .T. ) ;
#6738 = ORIENTED_EDGE ( 'NONE', *, *, #3919, .T. ) ;
#6739 = ADVANCED_FACE ( 'NONE', ( #1629 ), #3127, .F. ) ;
#6740 = CIRCLE ( 'NONE', #2289, 9.000000000000019540 ) ;
#6741 = AXIS2_PLACEMENT_3D ( 'NONE', #5802, #12025, #1121 ) ;
#6742 = CARTESIAN_POINT ( 'NONE',  ( 1.394999999999999574, -4.633866840648735774, -27.68468304288263582 ) ) ;
#6743 = CIRCLE ( 'NONE', #358, 8.800000000000022027 ) ;
#6744 = DIRECTION ( 'NONE',  ( 0.4999999999999945044, 0.8660254037844419273, -0.000000000000000000 ) ) ;
#6745 = CARTESIAN_POINT ( 'NONE',  ( -4.620319390059805187, 1.773574444220790136, -10.96874999795161720 ) ) ;
#6746 = VERTEX_POINT ( 'NONE', #16642 ) ;
#6747 = B_SPLINE_CURVE_WITH_KNOTS ( 'NONE', 3,
 ( #11232, #17236, #6608, #539, #12738, #3626 ),
 .UNSPECIFIED., .F., .F.,
 ( 4, 2, 4 ),
 ( 2.321268216996908089E-07, 0.001878622960950487733, 0.003757013795079275874 ),
 .UNSPECIFIED. ) ;
#6748 = DIRECTION ( 'NONE',  ( 0.000000000000000000, 0.000000000000000000, -1.000000000000000000 ) ) ;
#6749 = SHAPE_REPRESENTATION_RELATIONSHIP ( 'NONE' , 'NONE' ,  #4652, #1118 ) ;
#6751 = EDGE_CURVE ( 'NONE', #15630, #3846, #10353, .T. ) ;
#6750 = EDGE_CURVE ( 'NONE', #5745, #12101, #18900, .T. ) ;
#6752 = CARTESIAN_POINT ( 'NONE',  ( 0.8291131470075020493, -24.44424927289185590, 12.96989951879399072 ) ) ;
#6753 = EDGE_LOOP ( 'NONE', ( #1890, #3304 ) ) ;
#6754 = ORIENTED_EDGE ( 'NONE', *, *, #1271, .F. ) ;
#6755 = CARTESIAN_POINT ( 'NONE',  ( 5.207209108562820710, -2.318398865532073305, -14.00000000000000533 ) ) ;
#6756 = B_SPLINE_CURVE_WITH_KNOTS ( 'NONE', 3,
 ( #6505, #3519, #9636, #12730 ),
 .UNSPECIFIED., .F., .F.,
 ( 4, 4 ),
 ( 0.005258105385878687407, 0.005948373736081388405 ),
 .UNSPECIFIED. ) ;
#6757 = DIRECTION ( 'NONE',  ( -0.000000000000000000, -0.000000000000000000, -1.000000000000000000 ) ) ;
#6758 = CIRCLE ( 'NONE', #12852, 6.543750000000023270 ) ;
#6759 = CARTESIAN_POINT ( 'NONE',  ( 2.789999999999999147, -24.15498966839958683, -5.391175441198872598 ) ) ;
#6760 = AXIS2_PLACEMENT_3D ( 'NONE', #10867, #3255, #16878 ) ;
#6761 = VERTEX_POINT ( 'NONE', #1234 ) ;
#6762 = CARTESIAN_POINT ( 'NONE',  ( 0.000000000000000000, 0.000000000000000000, 29.00000000000000355 ) ) ;
#6763 = AXIS2_PLACEMENT_3D ( 'NONE', #4213, #13615, #2701 ) ;
#6764 = CARTESIAN_POINT ( 'NONE',  ( 13.00000000000000178, -3.830176896397409880, 3.037670790816764388 ) ) ;
#6765 = VERTEX_POINT ( 'NONE', #19640 ) ;
#6766 = LINE ( 'NONE', #3577, #12327 ) ;
#6767 = AXIS2_PLACEMENT_3D ( 'NONE', #598, #502, #6375 ) ;
#6768 = DIRECTION ( 'NONE',  ( -0.000000000000000000, 0.000000000000000000, 1.000000000000000000 ) ) ;
#6769 = CARTESIAN_POINT ( 'NONE',  ( 0.5279272933715204452, -19.66369668717018726, -18.56460150496961248 ) ) ;
#6770 = DIRECTION ( 'NONE',  ( 0.8660254037844417052, -0.4999999999999947820, 0.000000000000000000 ) ) ;
#6771 = CARTESIAN_POINT ( 'NONE',  ( -2.300000000000000711, 0.000000000000000000, 0.000000000000000000 ) ) ;
#6772 = CIRCLE ( 'NONE', #14145, 3.000000000000000000 ) ;
#6773 = CIRCLE ( 'NONE', #9354, 5.700000000000001954 ) ;
#6774 = DIRECTION ( 'NONE',  ( -1.000000000000000000, -0.000000000000000000, -0.000000000000000000 ) ) ;
#6775 = CARTESIAN_POINT ( 'NONE',  ( 2.789679245949058917, 20.70663861606308487, -12.51925356660738053 ) ) ;
#6776 = DIRECTION ( 'NONE',  ( 0.000000000000000000, 0.000000000000000000, 1.000000000000000000 ) ) ;
#6777 = ORIENTED_EDGE ( 'NONE', *, *, #2457, .F. ) ;
#6778 = FACE_OUTER_BOUND ( 'NONE', #8867, .T. ) ;
#6779 = CARTESIAN_POINT ( 'NONE',  ( -17.96448111170888851, 1.130229351527647585, 35.00000000000000000 ) ) ;
#6780 = UNCERTAINTY_MEASURE_WITH_UNIT (LENGTH_MEASURE( 1.000000000000000082E-05 ), #9507, 'distance_accuracy_value', 'NONE');
#6781 = LINE ( 'NONE', #19003, #11191 ) ;
#6782 = VECTOR ( 'NONE', #12457, 1000.000000000000000 ) ;
#6783 = DIRECTION ( 'NONE',  ( 0.000000000000000000, 0.000000000000000000, -1.000000000000000000 ) ) ;
#6784 = DIRECTION ( 'NONE',  ( 0.000000000000000000, 0.000000000000000000, -1.000000000000000000 ) ) ;
#6785 = CARTESIAN_POINT ( 'NONE',  ( -1.280903732194487166, -4.780397808154247308, -9.343749997951615427 ) ) ;
#6786 = VERTEX_POINT ( 'NONE', #19530 ) ;
#6787 = DIRECTION ( 'NONE',  ( -1.000000000000000000, 0.000000000000000000, 0.000000000000000000 ) ) ;
#6788 = CARTESIAN_POINT ( 'NONE',  ( 6.234374998975811266, 0.000000000000000000, -5.294050593750000644 ) ) ;
#6789 = AXIS2_PLACEMENT_3D ( 'NONE', #16361, #13263, #19353 ) ;
#6790 = VERTEX_POINT ( 'NONE', #13433 ) ;
#6791 = DIRECTION ( 'NONE',  ( 1.000000000000000000, 0.000000000000000000, 0.000000000000000000 ) ) ;
#6792 = CARTESIAN_POINT ( 'NONE',  ( -9.000000000000000000, 0.000000000000000000, -33.00000000000000000 ) ) ;
#6793 = AXIS2_PLACEMENT_3D ( 'NONE', #10555, #4739, #10656 ) ;
#6794 = MECHANICAL_DESIGN_GEOMETRIC_PRESENTATION_REPRESENTATION (  '', ( #6157 ), #17359 ) ;
#6795 = DIRECTION ( 'NONE',  ( 0.000000000000000000, 1.776356839400252831E-15, -1.000000000000000000 ) ) ;
#6796 =( BOUNDED_CURVE ( )  B_SPLINE_CURVE ( 2, ( #1824, #532, #12434, #14030, #18628, #6212, #5020, #9742, #4726, #11131, #17231 ),
 .UNSPECIFIED., .F., .F. ) 
 B_SPLINE_CURVE_WITH_KNOTS ( ( 3, 2, 2, 2, 2, 3 ),
 ( 0.1666819079834116757, 0.2000000000000000111, 0.2500000000000000000, 0.2999999999999999889, 0.3499999999999999778, 0.4000000000000000222 ),
 .UNSPECIFIED. ) 
 CURVE ( )  GEOMETRIC_REPRESENTATION_ITEM ( )  RATIONAL_B_SPLINE_CURVE ( ( 0.9945256517182512468, 0.9917959799814380917, 1.000000000000000000, 0.9876883405951377704, 1.000000000000000000, 0.9876883405951377704, 1.000000000000000000, 0.9876883405951377704, 1.000000000000000000, 0.9876883405951377704, 1.000000000000000000 ) ) 
 REPRESENTATION_ITEM ( '' )  );
#6797 = ORIENTED_EDGE ( 'NONE', *, *, #7445, .T. ) ;
#6798 = DIRECTION ( 'NONE',  ( 1.000000000000000000, 0.000000000000000000, 0.000000000000000000 ) ) ;
#6799 = FILL_AREA_STYLE ('',( #722 ) ) ;
#6800 = CARTESIAN_POINT ( 'NONE',  ( -2.500000000000002220, 9.887492094615969966E-16, 8.073750000000021743 ) ) ;
#6801 = EDGE_CURVE ( 'NONE', #15763, #488, #5824, .T. ) ;
#6802 = VERTEX_POINT ( 'NONE', #9038 ) ;
#6803 = CARTESIAN_POINT ( 'NONE',  ( 1.749999999999998002, 20.02152543075346003, 19.67366047555537634 ) ) ;
#6804 = ORIENTED_EDGE ( 'NONE', *, *, #18367, .T. ) ;
#6805 = CARTESIAN_POINT ( 'NONE',  ( 1.749999999999998002, 0.000000000000000000, 0.000000000000000000 ) ) ;
#6806 =( GEOMETRIC_REPRESENTATION_CONTEXT ( 3 ) GLOBAL_UNCERTAINTY_ASSIGNED_CONTEXT ( ( #3792 ) ) GLOBAL_UNIT_ASSIGNED_CONTEXT ( ( #10030, #1503, #12310 ) ) REPRESENTATION_CONTEXT ( 'NONE', 'WORKASPACE' ) );
#6807 = VERTEX_POINT ( 'NONE', #10445 ) ;
#6808 = CARTESIAN_POINT ( 'NONE',  ( 0.5321745326902582729, -3.467596033028097935, -26.83036154824997510 ) ) ;
#6809 = CARTESIAN_POINT ( 'NONE',  ( -2.620002426024544473, 5.142044285764750811, -10.81249999590322375 ) ) ;
#6810 = CARTESIAN_POINT ( 'NONE',  ( 10.58013454126452046, -14.56230589874905412, -32.00000000000000000 ) ) ;
#6811 = CARTESIAN_POINT ( 'NONE',  ( -3.490243377569957047E-16, 5.700000000000001066, -11.00000000000000711 ) ) ;
#6812 = ORIENTED_EDGE ( 'NONE', *, *, #17088, .T. ) ;
#6813 = CIRCLE ( 'NONE', #12900, 8.000000000000000000 ) ;
#6814 = FACE_BOUND ( 'NONE', #3134, .T. ) ;
#6815 = DIRECTION ( 'NONE',  ( 1.000000000000000000, 0.000000000000000000, 0.000000000000000000 ) ) ;
#6816 = EDGE_LOOP ( 'NONE', ( #10059, #3864, #18474, #12427 ) ) ;
#6817 = EDGE_CURVE ( 'NONE', #1977, #17754, #6107, .T. ) ;
#6818 =( GEOMETRIC_REPRESENTATION_CONTEXT ( 3 ) GLOBAL_UNCERTAINTY_ASSIGNED_CONTEXT ( ( #8591 ) ) GLOBAL_UNIT_ASSIGNED_CONTEXT ( ( #14093, #391, #4991 ) ) REPRESENTATION_CONTEXT ( 'NONE', 'WORKASPACE' ) );
#6819 = B_SPLINE_CURVE_WITH_KNOTS ( 'NONE', 3,
 ( #2401, #11513, #2205, #999 ),
 .UNSPECIFIED., .F., .F.,
 ( 4, 4 ),
 ( 2.324263106244727961E-07, 0.0006888201370294890283 ),
 .UNSPECIFIED. ) ;
#6820 = DIRECTION ( 'NONE',  ( -1.000000000000000000, 0.000000000000000000, 0.000000000000000000 ) ) ;
#6821 = CARTESIAN_POINT ( 'NONE',  ( 7.937500000000000000, 4.582717761692648217, -6.527800000000000047 ) ) ;
#6822 = CARTESIAN_POINT ( 'NONE',  ( 1.761396867937162769, -5.421022142882388373, -11.31249999590322375 ) ) ;
#6823 = VERTEX_POINT ( 'NONE', #15141 ) ;
#6824 = CARTESIAN_POINT ( 'NONE',  ( -7.937500000000000000, 0.000000000000000000, 0.000000000000000000 ) ) ;
#6825 = CARTESIAN_POINT ( 'NONE',  ( 0.000000000000000000, 0.000000000000000000, 0.000000000000000000 ) ) ;
#6826 = EDGE_CURVE ( 'NONE', #9896, #12690, #12044, .T. ) ;
#6827 = VECTOR ( 'NONE', #17787, 1000.000000000000000 ) ;
#6828 = ORIENTED_EDGE ( 'NONE', *, *, #6711, .T. ) ;
#6829 = CARTESIAN_POINT ( 'NONE',  ( 0.02436607992776151574, -18.55949924794880346, -16.37294372382878649 ) ) ;
#6830 = ORIENTED_EDGE ( 'NONE', *, *, #11474, .F. ) ;
#6831 = CARTESIAN_POINT ( 'NONE',  ( -30.00000000000000000, 4.400000000000000355, 0.000000000000000000 ) ) ;
#6832 = DIRECTION ( 'NONE',  ( 1.000000000000000000, 0.000000000000000000, 0.000000000000000000 ) ) ;
#6833 = DIRECTION ( 'NONE',  ( 0.000000000000000000, 0.000000000000000000, 1.000000000000000000 ) ) ;
#6834 = ORIENTED_EDGE ( 'NONE', *, *, #6398, .F. ) ;
#6835 = ORIENTED_EDGE ( 'NONE', *, *, #4310, .T. ) ;
#6836 = DIRECTION ( 'NONE',  ( -1.000000000000000000, -0.000000000000000000, -0.000000000000000000 ) ) ;
#6837 = CARTESIAN_POINT ( 'NONE',  ( 10.81249999590322375, -5.142044285764769462, 2.620002426024508502 ) ) ;
#6838 = CARTESIAN_POINT ( 'NONE',  ( 7.968749997951616315, 2.695436003842704764, 4.150607464521811174 ) ) ;
#6839 = VERTEX_POINT ( 'NONE', #18245 ) ;
#6840 = SURFACE_STYLE_USAGE ( .BOTH. , #5146 ) ;
#6841 = AXIS2_PLACEMENT_3D ( 'NONE', #15133, #1428, #13727 ) ;
#6842 = ADVANCED_FACE ( 'NONE', ( #3024 ), #14635, .F. ) ;
#6843 = EDGE_LOOP ( 'NONE', ( #19008, #15654, #951, #10598, #1572 ) ) ;
#6844 = EDGE_CURVE ( 'NONE', #4366, #13819, #6414, .T. ) ;
#6845 = FACE_OUTER_BOUND ( 'NONE', #10945, .T. ) ;
#6846 = CARTESIAN_POINT ( 'NONE',  ( 12.00000000000000533, -5.421022142882365280, -1.761396867937238042 ) ) ;
#6847 = EDGE_CURVE ( 'NONE', #10551, #9218, #7608, .T. ) ;
#6848 = CARTESIAN_POINT ( 'NONE',  ( -22.00000000000000355, 0.000000000000000000, -32.00000000000000000 ) ) ;
#6849 = AXIS2_PLACEMENT_3D ( 'NONE', #9604, #11000, #18894 ) ;
#6850 = ORIENTED_EDGE ( 'NONE', *, *, #7039, .F. ) ;
#6851 = ORIENTED_EDGE ( 'NONE', *, *, #7705, .T. ) ;
#6852 = CARTESIAN_POINT ( 'NONE',  ( -5.387740456496206143, 2.068159791354259092, -10.50000000000000711 ) ) ;
#6853 = ADVANCED_FACE ( 'NONE', ( #16141 ), #7001, .T. ) ;
#6854 = LINE ( 'NONE', #12982, #10953 ) ;
#6855 = VECTOR ( 'NONE', #14593, 1000.000000000000000 ) ;
#6856 = CARTESIAN_POINT ( 'NONE',  ( 0.006931038682727856497, -12.53626894672812853, -21.08061549536629187 ) ) ;
#6857 = ORIENTED_EDGE ( 'NONE', *, *, #14724, .F. ) ;
#6858 = CARTESIAN_POINT ( 'NONE',  ( 6.968749997951614539, -3.846120219227901149, -3.114526743279308896 ) ) ;
#6859 = CARTESIAN_POINT ( 'NONE',  ( 13.00000000000000888, -4.496324317583046515, -1.917446440021278731 ) ) ;
#6860 = EDGE_LOOP ( 'NONE', ( #13176, #9129, #3433, #2742, #15787, #6872 ) ) ;
#6861 = EDGE_CURVE ( 'NONE', #6695, #4912, #3726, .T. ) ;
#6862 = EDGE_CURVE ( 'NONE', #8877, #3117, #1655, .T. ) ;
#6863 = DIRECTION ( 'NONE',  ( 0.000000000000000000, 0.7806247497997995666, 0.6250000000000001110 ) ) ;
#6864 = DIRECTION ( 'NONE',  ( 1.000000000000000000, 0.000000000000000000, 0.000000000000000000 ) ) ;
#6865 = DIRECTION ( 'NONE',  ( -1.000000000000000000, -0.000000000000000000, -0.000000000000000000 ) ) ;
#6866 = FACE_OUTER_BOUND ( 'NONE', #19628, .T. ) ;
#6867 = AXIS2_PLACEMENT_3D ( 'NONE', #18247, #18053, #4527 ) ;
#6868 = CARTESIAN_POINT ( 'NONE',  ( 0.000000000000000000, -15.04425356660744839, -20.70663861606288236 ) ) ;
#6869 = CARTESIAN_POINT ( 'NONE',  ( -2.849999999999989431, 4.936344801571308061, -6.656249997951614539 ) ) ;
#6870 = AXIS2_PLACEMENT_3D ( 'NONE', #6514, #439, #332 ) ;
#6871 = CARTESIAN_POINT ( 'NONE',  ( 5.575441324182695446, 1.185096637661216201, -13.31249999590322730 ) ) ;
#6872 = ORIENTED_EDGE ( 'NONE', *, *, #11042, .T. ) ;
#6873 = DIRECTION ( 'NONE',  ( 0.000000000000000000, 0.000000000000000000, -1.000000000000000000 ) ) ;
#6874 = CARTESIAN_POINT ( 'NONE',  ( 18.11901729331276911, 5.562305898749055011, 32.00000000000000000 ) ) ;
#6875 = CARTESIAN_POINT ( 'NONE',  ( 1.886022603841227330, 1.012170579495290078E-15, 8.265000000000021885 ) ) ;
#6876 = ADVANCED_FACE ( 'NONE', ( #10040 ), #15936, .F. ) ;
#6877 = EDGE_CURVE ( 'NONE', #7268, #2962, #9747, .T. ) ;
#6878 = CARTESIAN_POINT ( 'NONE',  ( 12.84374999795161543, -1.016293382781378485, -4.781284448697201483 ) ) ;
#6879 = CARTESIAN_POINT ( 'NONE',  ( -1.886022603841296830, 0.000000000000000000, 0.000000000000000000 ) ) ;
#6880 = CARTESIAN_POINT ( 'NONE',  ( 0.2590123213420630899, -4.942249507334558700, -8.343749997951613651 ) ) ;
#6881 = ORIENTED_EDGE ( 'NONE', *, *, #14085, .T. ) ;
#6882 = CARTESIAN_POINT ( 'NONE',  ( 8.343749997951611874, -2.246813503491864150, 4.409619785863891472 ) ) ;
#6883 = DIRECTION ( 'NONE',  ( 0.000000000000000000, 3.552713678800500929E-15, 1.000000000000000000 ) ) ;
#6884 = EDGE_CURVE ( 'NONE', #15039, #9330, #3890, .T. ) ;
#6885 = CIRCLE ( 'NONE', #17467, 1.000000000000002665 ) ;
#6886 = ORIENTED_EDGE ( 'NONE', *, *, #10431, .F. ) ;
#6887 = LINE ( 'NONE', #13017, #7485 ) ;
#6888 = EDGE_CURVE ( 'NONE', #17830, #4459, #4533, .T. ) ;
#6889 = VECTOR ( 'NONE', #12026, 1000.000000000000000 ) ;
#6890 = CARTESIAN_POINT ( 'NONE',  ( 0.000000000000000000, 0.000000000000000000, 6.000000000000000000 ) ) ;
#6891 = CARTESIAN_POINT ( 'NONE',  ( 16.11901729331276556, 5.562305898749055011, -32.00000000000000000 ) ) ;
#6892 = CARTESIAN_POINT ( 'NONE',  ( -30.00000000000000000, 1.224646799147352468E-16, 0.000000000000000000 ) ) ;
#6893 = ORIENTED_EDGE ( 'NONE', *, *, #3422, .F. ) ;
#6894 = DIRECTION ( 'NONE',  ( 1.000000000000000000, 0.000000000000000000, 0.000000000000000000 ) ) ;
#6895 = DIRECTION ( 'NONE',  ( -1.000000000000000000, -0.000000000000000000, -0.000000000000000000 ) ) ;
#6896 = VERTEX_POINT ( 'NONE', #8527 ) ;
#6897 = DIRECTION ( 'NONE',  ( -1.000000000000000000, 0.000000000000000000, -0.000000000000000000 ) ) ;
#6898 = ORIENTED_EDGE ( 'NONE', *, *, #985, .T. ) ;
#6899 = CARTESIAN_POINT ( 'NONE',  ( 8.312499995903225525, -5.575441324182703440, 1.185096637661176677 ) ) ;
#6900 = CIRCLE ( 'NONE', #9480, 4.400000000000000355 ) ;
#6901 = ORIENTED_EDGE ( 'NONE', *, *, #7821, .T. ) ;
#6902 = CARTESIAN_POINT ( 'NONE',  ( 0.07181525068722535710, -2.576941577947229334, -25.22524549359953383 ) ) ;
#6903 = AXIS2_PLACEMENT_3D ( 'NONE', #17875, #2985, #3182 ) ;
#6904 = DIRECTION ( 'NONE',  ( 1.000000000000000000, 0.000000000000000000, 0.000000000000000000 ) ) ;
#6905 = ADVANCED_FACE ( 'NONE', ( #6607 ), #831, .T. ) ;
#6906 = CARTESIAN_POINT ( 'NONE',  ( -2.000000000000001776, 0.000000000000000000, 0.000000000000000000 ) ) ;
#6907 = DIRECTION ( 'NONE',  ( 1.000000000000000000, 0.000000000000000000, 0.000000000000000000 ) ) ;
#6908 = ORIENTED_EDGE ( 'NONE', *, *, #9173, .F. ) ;
#6909 = CARTESIAN_POINT ( 'NONE',  ( 2.030753603471114666, 12.98165646470082457, 24.32906614999620132 ) ) ;
#6910 = CARTESIAN_POINT ( 'NONE',  ( 12.31249999590322552, -2.850000000000023626, 4.936344801571289409 ) ) ;
#6911 = EDGE_LOOP ( 'NONE', ( #3561, #7917, #10246, #13836 ) ) ;
#6912 = ADVANCED_FACE ( 'NONE', ( #18928 ), #17965, .T. ) ;
#6913 =( BOUNDED_CURVE ( )  B_SPLINE_CURVE ( 2, ( #7481, #4592, #16605, #12198, #13698 ),
 .UNSPECIFIED., .F., .F. ) 
 B_SPLINE_CURVE_WITH_KNOTS ( ( 3, 2, 3 ),
 ( 0.3333180920165860761, 0.3499999999999999778, 0.4000000000000000222 ),
 .UNSPECIFIED. ) 
 CURVE ( )  GEOMETRIC_REPRESENTATION_ITEM ( )  RATIONAL_B_SPLINE_CURVE ( ( 0.9945256517182510247, 0.9958923606136991236, 1.000000000000000000, 0.9876883405951377704, 1.000000000000000000 ) ) 
 REPRESENTATION_ITEM ( '' )  );
#6914 = B_SPLINE_CURVE_WITH_KNOTS ( 'NONE', 1,
 ( #12174, #4961 ),
 .UNSPECIFIED., .F., .F.,
 ( 2, 2 ),
 ( 0.000000000000000000, 1.000000000000000000 ),
 .UNSPECIFIED. ) ;
#6915 = AXIS2_PLACEMENT_3D ( 'NONE', #6018, #8936, #2721 ) ;
#6916 =( REPRESENTATION_RELATIONSHIP ('NONE','NONE', #18211, #2588 ) REPRESENTATION_RELATIONSHIP_WITH_TRANSFORMATION ( #9868 )SHAPE_REPRESENTATION_RELATIONSHIP( ) );
#6917 = AXIS2_PLACEMENT_3D ( 'NONE', #9943, #17725, #19028 ) ;
#6918 = DIRECTION ( 'NONE',  ( 0.000000000000000000, 0.000000000000000000, 1.000000000000000000 ) ) ;
#6919 = CARTESIAN_POINT ( 'NONE',  ( 4.611396867937178179, -3.350375938067129855, -9.312499995903225525 ) ) ;
#6920 = VERTEX_POINT ( 'NONE', #632 ) ;
#6921 = FACE_OUTER_BOUND ( 'NONE', #5806, .T. ) ;
#6922 = ADVANCED_FACE ( 'NONE', ( #19126 ), #8326, .T. ) ;
#6923 = DIRECTION ( 'NONE',  ( 1.000000000000000000, 0.000000000000000000, 0.000000000000000000 ) ) ;
#6924 = FACE_BOUND ( 'NONE', #17909, .T. ) ;
#6925 = EDGE_LOOP ( 'NONE', ( #12040, #18684 ) ) ;
#6926 = CYLINDRICAL_SURFACE ( 'NONE', #6190, 13.19999999999999929 ) ;
#6927 = ORIENTED_EDGE ( 'NONE', *, *, #5636, .T. ) ;
#6928 = PLANE ( 'NONE',  #16382 ) ;
#6929 = DIRECTION ( 'NONE',  ( 0.000000000000000000, 0.000000000000000000, 1.000000000000000000 ) ) ;
#6930 = DIRECTION ( 'NONE',  ( 0.000000000000000000, 0.000000000000000000, 1.000000000000000000 ) ) ;
#6931 = EDGE_LOOP ( 'NONE', ( #6487, #8119, #2632, #4055 ) ) ;
#6932 = FACE_OUTER_BOUND ( 'NONE', #18768, .T. ) ;
#6933 = DIRECTION ( 'NONE',  ( -1.000000000000000000, 0.000000000000000000, 0.000000000000000000 ) ) ;
#6934 = AXIS2_PLACEMENT_3D ( 'NONE', #2021, #15437, #4825 ) ;
#6935 = LINE ( 'NONE', #19246, #6288 ) ;
#6936 = AXIS2_PLACEMENT_3D ( 'NONE', #12665, #8646, #8846 ) ;
#6937 = ORIENTED_EDGE ( 'NONE', *, *, #15988, .F. ) ;
#6938 = EDGE_CURVE ( 'NONE', #4210, #14047, #5222, .T. ) ;
#6939 = DIRECTION ( 'NONE',  ( 0.000000000000000000, 0.000000000000000000, 1.000000000000000000 ) ) ;
#6940 = VERTEX_POINT ( 'NONE', #12935 ) ;
#6941 = CARTESIAN_POINT ( 'NONE',  ( 2.030753605846571386, 27.31305418910209326, 3.797885586973312133 ) ) ;
#6942 = CIRCLE ( 'NONE', #14643, 6.735000000000022524 ) ;
#6943 = PLANE ( 'NONE',  #13835 ) ;
#6944 = ORIENTED_EDGE ( 'NONE', *, *, #4890, .F. ) ;
#6945 = CARTESIAN_POINT ( 'NONE',  ( 0.000000000000000000, 0.000000000000000000, -35.00000000000000000 ) ) ;
#6946 = SURFACE_STYLE_USAGE ( .BOTH. , #3965 ) ;
#6947 = CARTESIAN_POINT ( 'NONE',  ( 1.039999999999996039, 27.68468304288258963, 4.633866840649018215 ) ) ;
#6948 = VERTEX_POINT ( 'NONE', #15736 ) ;
#6949 = EDGE_CURVE ( 'NONE', #14221, #17740, #14762, .T. ) ;
#6950 = ADVANCED_FACE ( 'NONE', ( #11434 ), #717, .T. ) ;
#6951 = ORIENTED_EDGE ( 'NONE', *, *, #6938, .F. ) ;
#6952 = CARTESIAN_POINT ( 'NONE',  ( 2.783068888626320625, -9.685942809246897767, -22.53293026234513619 ) ) ;
#6953 = DIRECTION ( 'NONE',  ( 1.000000000000000000, 0.000000000000000000, 0.000000000000000000 ) ) ;
#6954 = CIRCLE ( 'NONE', #8888, 9.000000000000000000 ) ;
#6955 = CARTESIAN_POINT ( 'NONE',  ( -1.899999999999999023, 0.000000000000000000, 0.000000000000000000 ) ) ;
#6956 = AXIS2_PLACEMENT_3D ( 'NONE', #19591, #18295, #14897 ) ;
#6957 = ORIENTED_EDGE ( 'NONE', *, *, #5900, .T. ) ;
#6958 = ADVANCED_FACE ( 'NONE', ( #18030 ), #10130, .F. ) ;
#6959 = DIRECTION ( 'NONE',  ( -0.000000000000000000, -0.000000000000000000, 1.000000000000000000 ) ) ;
#6960 = DIRECTION ( 'NONE',  ( 0.000000000000000000, 0.000000000000000000, 1.000000000000000000 ) ) ;
#6961 = ORIENTED_EDGE ( 'NONE', *, *, #6240, .F. ) ;
#6962 = DIRECTION ( 'NONE',  ( 0.000000000000000000, 0.000000000000000000, -1.000000000000000000 ) ) ;
#6963 = FACE_BOUND ( 'NONE', #19273, .T. ) ;
#6964 = FACE_OUTER_BOUND ( 'NONE', #6537, .T. ) ;
#6965 = CARTESIAN_POINT ( 'NONE',  ( 10.84374999795161543, 3.632567103900524064, 3.270778111535338262 ) ) ;
#6966 = PRODUCT_DEFINITION_SHAPE ( 'NONE', 'NONE',  #19788 ) ;
#6967 = CIRCLE ( 'NONE', #5687, 1.000000000000003553 ) ;
#6968 = DIRECTION ( 'NONE',  ( 0.000000000000000000, 0.000000000000000000, 1.000000000000000000 ) ) ;
#6969 = LINE ( 'NONE', #19183, #4865 ) ;
#6970 = ORIENTED_EDGE ( 'NONE', *, *, #11649, .T. ) ;
#6971 = CYLINDRICAL_SURFACE ( 'NONE', #15919, 8.000000000000000000 ) ;
#6972 = CARTESIAN_POINT ( 'NONE',  ( -4.465502636338010589, 1.988169868018623720, -14.46874999795161720 ) ) ;
#6973 = UNCERTAINTY_MEASURE_WITH_UNIT (LENGTH_MEASURE( 1.000000000000000082E-05 ), #15700, 'distance_accuracy_value', 'NONE');
#6974 = CARTESIAN_POINT ( 'NONE',  ( 0.5109457054261454800, -4.861323657744410554, -14.84374999795161543 ) ) ;
#6975 = AXIS2_PLACEMENT_3D ( 'NONE', #11858, #10467, #10271 ) ;
#6976 = DIRECTION ( 'NONE',  ( 0.000000000000000000, 0.000000000000000000, 1.000000000000000000 ) ) ;
#6977 = DIRECTION ( 'NONE',  ( 0.000000000000000000, 0.000000000000000000, 1.000000000000000000 ) ) ;
#6978 = VERTEX_POINT ( 'NONE', #17726 ) ;
#6979 = EDGE_CURVE ( 'NONE', #639, #3073, #5997, .T. ) ;
#6980 = FACE_OUTER_BOUND ( 'NONE', #11078, .T. ) ;
#6981 = EDGE_CURVE ( 'NONE', #8643, #13582, #12020, .T. ) ;
#6982 = CYLINDRICAL_SURFACE ( 'NONE', #19060, 1.000000000000000888 ) ;
#6983 = VECTOR ( 'NONE', #4526, 1000.000000000000000 ) ;
#6984 = ORIENTED_EDGE ( 'NONE', *, *, #7571, .F. ) ;
#6985 = DIRECTION ( 'NONE',  ( -0.000000000000000000, -0.000000000000000000, 1.000000000000000000 ) ) ;
#6986 = DIRECTION ( 'NONE',  ( 0.000000000000000000, 0.000000000000000000, -1.000000000000000000 ) ) ;
#6987 = B_SPLINE_CURVE_WITH_KNOTS ( 'NONE', 3,
 ( #16028, #13030, #19123, #5413, #17627, #14820, #1210, #2602 ),
 .UNSPECIFIED., .F., .F.,
 ( 4, 2, 2, 4 ),
 ( 0.004637198101876872751, 0.005792104118025187022, 0.006947010134173500426, 0.009256822166470130703 ),
 .UNSPECIFIED. ) ;
#6988 = DIRECTION ( 'NONE',  ( -0.8660254037844399289, -0.4999999999999978906, 0.000000000000000000 ) ) ;
#6989 = DIRECTION ( 'NONE',  ( -1.000000000000000000, 0.000000000000000000, 0.000000000000000000 ) ) ;
#6990 = EDGE_CURVE ( 'NONE', #2257, #3690, #10921, .T. ) ;
#6991 = VERTEX_POINT ( 'NONE', #7388 ) ;
#6992 = CARTESIAN_POINT ( 'NONE',  ( 10.12500000000000178, 0.000000000000000000, 4.000000000000000000 ) ) ;
#6993 = CARTESIAN_POINT ( 'NONE',  ( -2.849999999999988987, 4.936344801571308061, -6.000000000000005329 ) ) ;
#6994 = DIRECTION ( 'NONE',  ( 0.000000000000000000, 0.000000000000000000, 1.000000000000000000 ) ) ;
#6995 = EDGE_LOOP ( 'NONE', ( #2252, #11370, #4868, #3956 ) ) ;
#6996 = CARTESIAN_POINT ( 'NONE',  ( 9.812499995903225525, -5.574407415329147852, -1.493657965219562511 ) ) ;
#6997 = ORIENTED_EDGE ( 'NONE', *, *, #15052, .F. ) ;
#6998 = EDGE_CURVE ( 'NONE', #3097, #7592, #9014, .T. ) ;
#6999 = CARTESIAN_POINT ( 'NONE',  ( 0.02436607992775717893, -9.836394144775869819, 22.71065055754449347 ) ) ;
#7000 = CARTESIAN_POINT ( 'NONE',  ( 0.006974657972266078837, 5.408388659524427489, -23.92335783895632417 ) ) ;
#7001 = CYLINDRICAL_SURFACE ( 'NONE', #17622, 22.00000000000000355 ) ;
#7002 = CIRCLE ( 'NONE', #12141, 5.700000000000001954 ) ;
#7003 = PLANE ( 'NONE',  #5677 ) ;
#7004 = ORIENTED_EDGE ( 'NONE', *, *, #17208, .T. ) ;
#7005 = FACE_BOUND ( 'NONE', #15215, .T. ) ;
#7006 = DIRECTION ( 'NONE',  ( -1.000000000000000000, 0.000000000000000000, 0.000000000000000000 ) ) ;
#7007 = VERTEX_POINT ( 'NONE', #16228 ) ;
#7008 = EDGE_CURVE ( 'NONE', #2089, #8012, #9770, .T. ) ;
#7009 = DIRECTION ( 'NONE',  ( -1.000000000000000000, 0.000000000000000000, -0.000000000000000000 ) ) ;
#7010 = LINE ( 'NONE', #5522, #10970 ) ;
#7011 = ORIENTED_EDGE ( 'NONE', *, *, #5451, .T. ) ;
#7013 = CARTESIAN_POINT ( 'NONE',  ( 5.366045694719498695E-16, 9.514945144209063344, -22.37986894186662923 ) ) ;
#7012 = CIRCLE ( 'NONE', #6368, 24.12539914357697413 ) ;
#7014 = FACE_OUTER_BOUND ( 'NONE', #11149, .T. ) ;
#7015 = AXIS2_PLACEMENT_3D ( 'NONE', #7913, #17131, #17228 ) ;
#7016 = DIRECTION ( 'NONE',  ( 0.000000000000000000, 0.000000000000000000, 1.000000000000000000 ) ) ;
#7017 = EDGE_LOOP ( 'NONE', ( #15486, #4008, #6084, #14742 ) ) ;
#7018 = DIRECTION ( 'NONE',  ( 0.000000000000000000, 1.000000000000000000, 0.000000000000000000 ) ) ;
#7019 = ORIENTED_EDGE ( 'NONE', *, *, #3666, .T. ) ;
#7020 = CARTESIAN_POINT ( 'NONE',  ( 8.000000000000000000, -2.000000000000002665, 41.99999999999999289 ) ) ;
#7021 = PRESENTATION_STYLE_ASSIGNMENT (( #14459 ) ) ;
#7022 = DIRECTION ( 'NONE',  ( 0.000000000000000000, 0.000000000000000000, 1.000000000000000000 ) ) ;
#7023 = ORIENTED_EDGE ( 'NONE', *, *, #16502, .F. ) ;
#7024 = CARTESIAN_POINT ( 'NONE',  ( -1.255998204157475318, -17.85806462366060288, -32.00000000000000000 ) ) ;
#7025 = DIRECTION ( 'NONE',  ( 1.000000000000000000, 0.000000000000000000, 0.000000000000000000 ) ) ;
#7026 = CARTESIAN_POINT ( 'NONE',  ( 2.000000000000000000, 1.999999999999997335, 37.99999999999999289 ) ) ;
#7027 = ORIENTED_EDGE ( 'NONE', *, *, #10838, .T. ) ;
#7028 =( BOUNDED_CURVE ( )  B_SPLINE_CURVE ( 2, ( #16864, #12260, #4356, #18066, #18359, #13449, #14962, #8957, #19752, #4653, #7537, #9060, #15265, #3147, #18168, #19551, #1158 ),
 .UNSPECIFIED., .F., .F. ) 
 B_SPLINE_CURVE_WITH_KNOTS ( ( 3, 2, 2, 2, 2, 2, 2, 2, 3 ),
 ( 0.000000000000000000, 0.05000000000000000971, 0.1000000000000000194, 0.1499999999999999944, 0.2000000000000000389, 0.2500000000000000000, 0.2999999999999999889, 0.3499999999999999223, 0.4000000000000000777 ),
 .UNSPECIFIED. ) 
 CURVE ( )  GEOMETRIC_REPRESENTATION_ITEM ( )  RATIONAL_B_SPLINE_CURVE ( ( 1.000000000000000000, 0.9876883405951377704, 1.000000000000000000, 0.9876883405951377704, 1.000000000000000000, 0.9876883405951377704, 1.000000000000000000, 0.9876883405951377704, 1.000000000000000000, 0.9876883405951377704, 1.000000000000000000, 0.9876883405951377704, 1.000000000000000000, 0.9876883405951377704, 1.000000000000000000, 0.9876883405951377704, 1.000000000000000000 ) ) 
 REPRESENTATION_ITEM ( '' )  );
#7029 = VECTOR ( 'NONE', #16696, 1000.000000000000000 ) ;
#7030 = VECTOR ( 'NONE', #9111, 999.9999999999998863 ) ;
#7031 = DIRECTION ( 'NONE',  ( -0.8660254037844398178, 0.000000000000000000, 0.4999999999999979461 ) ) ;
#7032 = VERTEX_POINT ( 'NONE', #7290 ) ;
#7033 = CARTESIAN_POINT ( 'NONE',  ( 13.00000000000000000, 0.2080849974989116558, 4.883670121236158401 ) ) ;
#7034 = DIRECTION ( 'NONE',  ( -1.000000000000000000, 0.000000000000000000, -0.000000000000000000 ) ) ;
#7035 = VERTEX_POINT ( 'NONE', #10423 ) ;
#7036 = CARTESIAN_POINT ( 'NONE',  ( -3.632567103900569361, -3.270778111535287191, -7.843749997951614539 ) ) ;
#7037 = VECTOR ( 'NONE', #4297, 1000.000000000000000 ) ;
#7038 = CARTESIAN_POINT ( 'NONE',  ( 3.255998204157476206, -17.85806462366060288, -35.00000000000000000 ) ) ;
#7039 = EDGE_CURVE ( 'NONE', #2859, #17179, #13227, .T. ) ;
#7040 = EDGE_LOOP ( 'NONE', ( #12007, #3745, #8744, #3172 ) ) ;
#7041 = ORIENTED_EDGE ( 'NONE', *, *, #1295, .T. ) ;
#7042 = DIRECTION ( 'NONE',  ( 0.000000000000000000, 0.000000000000000000, 1.000000000000000000 ) ) ;
#7043 = CARTESIAN_POINT ( 'NONE',  ( 1.998465710409312357E-16, 22.37986894186671805, 9.514945144208807548 ) ) ;
#7044 = ORIENTED_EDGE ( 'NONE', *, *, #12130, .T. ) ;
#7045 = CARTESIAN_POINT ( 'NONE',  ( 0.000000000000000000, -12.52067188844335988, -20.62201879784928238 ) ) ;
#7046 = ORIENTED_EDGE ( 'NONE', *, *, #4312, .F. ) ;
#7047 = CARTESIAN_POINT ( 'NONE',  ( 112.0000000000000000, 4.484350416777816686E-16, -3.323499999999993015 ) ) ;
#7048 = FACE_OUTER_BOUND ( 'NONE', #8160, .T. ) ;
#7049 = CIRCLE ( 'NONE', #1635, 28.06981291497571362 ) ;
#7050 = EDGE_LOOP ( 'NONE', ( #15436, #2878, #2364, #4226 ) ) ;
#7051 = CARTESIAN_POINT ( 'NONE',  ( 0.000000000000000000, 0.000000000000000000, -0.5557897334539606549 ) ) ;
#7052 = CIRCLE ( 'NONE', #6106, 4.200000000000000178 ) ;
#7053 = ADVANCED_FACE ( 'NONE', ( #7192 ), #10330, .T. ) ;
#7054 = B_SPLINE_CURVE_WITH_KNOTS ( 'NONE', 3,
 ( #10509, #8903, #4492, #10603, #13798, #12201 ),
 .UNSPECIFIED., .F., .F.,
 ( 4, 2, 4 ),
 ( 2.380731676726218893E-07, 0.002318718087522284119, 0.004637198101876895302 ),
 .UNSPECIFIED. ) ;
#7055 = B_SPLINE_CURVE_WITH_KNOTS ( 'NONE', 1,
 ( #5761, #7456 ),
 .UNSPECIFIED., .F., .F.,
 ( 2, 2 ),
 ( 0.000000000000000000, 1.000000000000000000 ),
 .UNSPECIFIED. ) ;
#7056 = DIRECTION ( 'NONE',  ( 0.000000000000000000, 0.000000000000000000, -1.000000000000000000 ) ) ;
#7057 = CARTESIAN_POINT ( 'NONE',  ( 5.313169144388799836, 6.097875887622421054, -0.08160424337823990459 ) ) ;
#7058 = DIRECTION ( 'NONE',  ( 0.000000000000000000, 0.000000000000000000, 1.000000000000000000 ) ) ;
#7059 = DIRECTION ( 'NONE',  ( -0.000000000000000000, -0.000000000000000000, 1.000000000000000000 ) ) ;
#7060 = CARTESIAN_POINT ( 'NONE',  ( 2.790000000000076863, -12.51293083811783191, -20.85287692521943015 ) ) ;
#7061 = EDGE_CURVE ( 'NONE', #9260, #6039, #1338, .T. ) ;
#7062 = EDGE_LOOP ( 'NONE', ( #15932, #17775, #7401, #10162 ) ) ;
#7063 = CARTESIAN_POINT ( 'NONE',  ( 0.000000000000000000, 0.000000000000000000, 0.000000000000000000 ) ) ;
#7064 = AXIS2_PLACEMENT_3D ( 'NONE', #16835, #16732, #6108 ) ;
#7065 = DIRECTION ( 'NONE',  ( 0.000000000000000000, 0.000000000000000000, -1.000000000000000000 ) ) ;
#7066 = CIRCLE ( 'NONE', #48, 6.200000000000021494 ) ;
#7067 = DIRECTION ( 'NONE',  ( 1.000000000000000000, 0.000000000000000000, -0.000000000000000000 ) ) ;
#7068 = CARTESIAN_POINT ( 'NONE',  ( 3.270778111535314281, -3.632567103900546712, -12.46874999795161543 ) ) ;
#7069 = ORIENTED_EDGE ( 'NONE', *, *, #134, .T. ) ;
#7070 = CARTESIAN_POINT ( 'NONE',  ( 0.1855654851361725199, -23.63475234378974577, -10.67816411292190004 ) ) ;
#7071 = AXIS2_PLACEMENT_3D ( 'NONE', #4898, #11301, #6472 ) ;
#7072 = CARTESIAN_POINT ( 'NONE',  ( 4.840010801796506001, 3.143139765844590983, -8.812499995903225525 ) ) ;
#7073 = EDGE_LOOP ( 'NONE', ( #3190, #3777, #3593, #6944 ) ) ;
#7074 = ADVANCED_FACE ( 'NONE', ( #8617 ), #8040, .T. ) ;
#7076 = FACE_OUTER_BOUND ( 'NONE', #18119, .T. ) ;
#7075 = ADVANCED_BREP_SHAPE_REPRESENTATION ( '', ( #15810, #16724 ), #17389 ) ;
#7077 = AXIS2_PLACEMENT_3D ( 'NONE', #11974, #19270, #14977 ) ;
#7078 = AXIS2_PLACEMENT_3D ( 'NONE', #2270, #15587, #6655 ) ;
#7079 = DIRECTION ( 'NONE',  ( -1.000000000000000000, -0.000000000000000000, -0.000000000000000000 ) ) ;
#7080 = CARTESIAN_POINT ( 'NONE',  ( 2.765633920072235963, 22.71065055754452544, 9.836394144775786330 ) ) ;
#7081 = EDGE_CURVE ( 'NONE', #1705, #12785, #17861, .T. ) ;
#7082 = EDGE_LOOP ( 'NONE', ( #5948, #14096, #9498, #16301 ) ) ;
#7083 = LINE ( 'NONE', #15824, #12669 ) ;
#7084 = LINE ( 'NONE', #17621, #142 ) ;
#7085 = CIRCLE ( 'NONE', #7751, 24.12539914357697768 ) ;
#7086 = CARTESIAN_POINT ( 'NONE',  ( 7.500000000000005329, -2.620002426024580000, 5.142044285764733935 ) ) ;
#7087 = EDGE_LOOP ( 'NONE', ( #10963, #15149, #15037, #9160 ) ) ;
#7088 = ADVANCED_FACE ( 'NONE', ( #13314 ), #15119, .F. ) ;
#7089 = CARTESIAN_POINT ( 'NONE',  ( 2.790000000000077751, 5.456611084821854085, 23.69897269326679279 ) ) ;
#7090 = ORIENTED_EDGE ( 'NONE', *, *, #17291, .F. ) ;
#7091 = FACE_BOUND ( 'NONE', #9946, .T. ) ;
#7092 = CARTESIAN_POINT ( 'NONE',  ( 0.02436607992776194942, -5.391175441198450713, -24.15498966839968276 ) ) ;
#7093 = CARTESIAN_POINT ( 'NONE',  ( 1.394999999999999574, -19.67366047555544739, 20.02152543075338897 ) ) ;
#7094 = AXIS2_PLACEMENT_3D ( 'NONE', #13975, #13773, #1961 ) ;
#7095 = CARTESIAN_POINT ( 'NONE',  ( 4.080749450109649956, 4.080749450109650844, -13.50000000000000533 ) ) ;
#7096 = VERTEX_POINT ( 'NONE', #10520 ) ;
#7097 = VECTOR ( 'NONE', #11571, 1000.000000000000000 ) ;
#7098 = CARTESIAN_POINT ( 'NONE',  ( 6.843749997951615427, -3.413342815706642518E-14, 4.888101187500000222 ) ) ;
#7099 = EDGE_CURVE ( 'NONE', #5891, #6823, #14115, .T. ) ;
#7100 = DIRECTION ( 'NONE',  ( 0.000000000000000000, 0.000000000000000000, -1.000000000000000000 ) ) ;
#7101 = ORIENTED_EDGE ( 'NONE', *, *, #12099, .F. ) ;
#7102 = VECTOR ( 'NONE', #2839, 1000.000000000000000 ) ;
#7103 = CIRCLE ( 'NONE', #1056, 2.524999999999995914 ) ;
#7104 = EDGE_CURVE ( 'NONE', #19695, #2660, #15253, .T. ) ;
#7105 = DIRECTION ( 'NONE',  ( -0.000000000000000000, 0.000000000000000000, 1.000000000000000000 ) ) ;
#7106 = CARTESIAN_POINT ( 'NONE',  ( 0.000000000000000000, -20.62201879784905501, -12.52067188844372936 ) ) ;
#7107 = EDGE_LOOP ( 'NONE', ( #6350, #14654 ) ) ;
#7108 =( GEOMETRIC_REPRESENTATION_CONTEXT ( 3 ) GLOBAL_UNCERTAINTY_ASSIGNED_CONTEXT ( ( #14406 ) ) GLOBAL_UNIT_ASSIGNED_CONTEXT ( ( #17225, #3713, #9737 ) ) REPRESENTATION_CONTEXT ( 'NONE', 'WORKASPACE' ) );
#7109 = CARTESIAN_POINT ( 'NONE',  ( 13.00000000000000533, 5.207209108562852684, -2.318398865532001363 ) ) ;
#7110 = CARTESIAN_POINT ( 'NONE',  ( -1.761396867937238042, -5.421022142882365280, -12.00000000000000533 ) ) ;
#7111 = CARTESIAN_POINT ( 'NONE',  ( 7.968749997951616315, 2.246813503491833508, -4.409619785863906571 ) ) ;
#7112 = VERTEX_POINT ( 'NONE', #14922 ) ;
#7113 = CARTESIAN_POINT ( 'NONE',  ( 0.1855655959470668692, 17.45907811351482763, -19.17825124759758282 ) ) ;
#7114 = VERTEX_POINT ( 'NONE', #1212 ) ;
#7115 = CARTESIAN_POINT ( 'NONE',  ( 2.789999999999999147, -24.44424927289185590, 12.96989951879399072 ) ) ;
#7116 = ORIENTED_EDGE ( 'NONE', *, *, #4214, .F. ) ;
#7117 = EDGE_CURVE ( 'NONE', #8320, #15591, #8915, .T. ) ;
#7118 = DIRECTION ( 'NONE',  ( 0.000000000000000000, 0.000000000000000000, -1.000000000000000000 ) ) ;
#7119 = CARTESIAN_POINT ( 'NONE',  ( -20.63749999999999929, 0.000000000000000000, 0.000000000000000000 ) ) ;
#7120 = AXIS2_PLACEMENT_3D ( 'NONE', #8312, #19202, #8606 ) ;
#7121 = DIRECTION ( 'NONE',  ( 1.000000000000000000, 0.000000000000000000, 0.000000000000000000 ) ) ;
#7122 = ORIENTED_EDGE ( 'NONE', *, *, #4603, .F. ) ;
#7123 = CARTESIAN_POINT ( 'NONE',  ( -0.7741991708319226895, -4.888101187499994893, -12.34374999795161543 ) ) ;
#7124 = CARTESIAN_POINT ( 'NONE',  ( 7.937500000000000000, 4.582717761692648217, -6.527800000000000047 ) ) ;
#7125 = CARTESIAN_POINT ( 'NONE',  ( 0.000000000000000000, 0.000000000000000000, 0.000000000000000000 ) ) ;
#7126 = EDGE_LOOP ( 'NONE', ( #335, #1, #14857, #4332 ) ) ;
#7127 = EDGE_CURVE ( 'NONE', #18731, #17165, #9256, .T. ) ;
#7128 = COLOUR_RGB ( '', 0.08235294, 0.09019608, 0.10196078) ;
#7129 = DIRECTION ( 'NONE',  ( 1.000000000000000000, 0.000000000000000000, 0.000000000000000000 ) ) ;
#7130 = PRODUCT_DEFINITION_SHAPE ( 'NONE', 'NONE',  #19796 ) ;
#7131 = EDGE_LOOP ( 'NONE', ( #6908, #9425, #11251, #589 ) ) ;
#7132 = VECTOR ( 'NONE', #7881, 1000.000000000000000 ) ;
#7133 = CARTESIAN_POINT ( 'NONE',  ( 0.02436607992775978102, 16.37294372382885044, -18.55949924794875017 ) ) ;
#7134 = DIRECTION ( 'NONE',  ( 0.000000000000000000, 1.000000000000000000, 0.000000000000000000 ) ) ;
#7135 = ORIENTED_EDGE ( 'NONE', *, *, #19103, .F. ) ;
#7136 = DIRECTION ( 'NONE',  ( -1.000000000000000000, -0.000000000000000000, -0.000000000000000000 ) ) ;
#7137 = AXIS2_PLACEMENT_3D ( 'NONE', #18284, #10682, #19678 ) ;
#7138 = FACE_OUTER_BOUND ( 'NONE', #2194, .T. ) ;
#7139 = EDGE_LOOP ( 'NONE', ( #13216, #10976, #853, #16176, #7459, #8499, #4566, #11971, #7358, #3711, #2935, #14709, #13370, #4925, #19022, #19411, #17279, #15960, #12520, #10578, #7390, #339, #18325, #13093, #12089, #523, #3742, #12075, #11543, #11496, #17171, #5019, #9196, #18025, #2043, #9154, #11218, #3975, #215, #1811, #3146, #11921, #661, #12589, #7661 ) ) ;
#7140 = ORIENTED_EDGE ( 'NONE', *, *, #12182, .T. ) ;
#7141 = LINE ( 'NONE', #5654, #4740 ) ;
#7142 = LINE ( 'NONE', #16476, #11425 ) ;
#7143 = ADVANCED_FACE ( 'NONE', ( #18319 ), #3201, .F. ) ;
#7145 = EDGE_LOOP ( 'NONE', ( #6141, #4720 ) ) ;
#7144 = VECTOR ( 'NONE', #1302, 1000.000000000000000 ) ;
#7146 = FACE_OUTER_BOUND ( 'NONE', #18312, .T. ) ;
#7147 = ORIENTED_EDGE ( 'NONE', *, *, #4199, .T. ) ;
#7148 = DIRECTION ( 'NONE',  ( -1.000000000000000000, 0.000000000000000000, 0.000000000000000000 ) ) ;
#7149 = CARTESIAN_POINT ( 'NONE',  ( 13.00000000000000178, -4.390212428369197006, -2.150226904532469341 ) ) ;
#7150 = AXIS2_PLACEMENT_3D ( 'NONE', #8656, #16079, #11374 ) ;
#7151 = ORIENTED_EDGE ( 'NONE', *, *, #2405, .T. ) ;
#7152 = DIRECTION ( 'NONE',  ( 0.000000000000000000, 0.000000000000000000, -1.000000000000000000 ) ) ;
#7153 = ADVANCED_FACE ( 'NONE', ( #14106 ), #18224, .T. ) ;
#7154 = DIRECTION ( 'NONE',  ( 0.000000000000000000, 0.000000000000000000, 1.000000000000000000 ) ) ;
#7155 = CARTESIAN_POINT ( 'NONE',  ( 14.34374999795161365, 3.499494075959816541, 3.499494075959815653 ) ) ;
#7156 = CARTESIAN_POINT ( 'NONE',  ( 9.843749997951615427, 4.465502636338024800, 1.988169868018593300 ) ) ;
#7157 = ADVANCED_FACE ( 'NONE', ( #16723 ), #404, .F. ) ;
#7158 = CARTESIAN_POINT ( 'NONE',  ( 0.000000000000000000, 0.000000000000000000, 0.000000000000000000 ) ) ;
#7159 =( NAMED_UNIT ( * ) PLANE_ANGLE_UNIT ( ) SI_UNIT ( $, .RADIAN. ) );
#7160 = DIRECTION ( 'NONE',  ( 0.000000000000000000, 0.000000000000000000, 1.000000000000000000 ) ) ;
#7161 = EDGE_LOOP ( 'NONE', ( #11067, #14422, #19470, #18648 ) ) ;
#7162 = CARTESIAN_POINT ( 'NONE',  ( 2.789999999999999147, 7.909232158575156824, -24.34211360614291664 ) ) ;
#7163 = AXIS2_PLACEMENT_3D ( 'NONE', #3031, #15450, #4442 ) ;
#7164 = CARTESIAN_POINT ( 'NONE',  ( 0.0003207540509378258692, 20.70663861606293921, -12.51925356660738053 ) ) ;
#7165 = UNCERTAINTY_MEASURE_WITH_UNIT (LENGTH_MEASURE( 1.000000000000000082E-05 ), #5847, 'distance_accuracy_value', 'NONE');
#7166 = CARTESIAN_POINT ( 'NONE',  ( -1.493657965219446160, 5.574407415329178939, -13.50000000000000533 ) ) ;
#7167 = LINE ( 'NONE', #5678, #12867 ) ;
#7168 = CARTESIAN_POINT ( 'NONE',  ( -4.888101187500000222, 0.7741991708318887166, -7.343749997951615427 ) ) ;
#7169 = EDGE_LOOP ( 'NONE', ( #7293, #7939, #11548, #7849, #5505, #4673, #15272, #11913, #4398, #14646, #6881, #14144, #11143, #13501, #7212, #14581, #4105, #8728, #9759, #15577, #9789, #848, #14212, #9881, #4523, #1133, #12517, #12241, #12862, #12275, #1032, #11650, #5352, #9688, #16455, #15714, #19262, #7116, #8651, #7046, #11450, #5884, #4134, #16417, #3630 ) ) ;
#7170 = DIRECTION ( 'NONE',  ( 0.000000000000000000, 0.000000000000000000, 1.000000000000000000 ) ) ;
#7171 = CARTESIAN_POINT ( 'NONE',  ( 0.1882238946918237121, 25.78859396478527799, -2.857713464478781162 ) ) ;
#7172 = VERTEX_POINT ( 'NONE', #3406 ) ;
#7173 = CARTESIAN_POINT ( 'NONE',  ( -20.63749999999999929, 0.000000000000000000, 0.000000000000000000 ) ) ;
#7174 = EDGE_CURVE ( 'NONE', #10470, #10657, #18279, .T. ) ;
#7175 = CARTESIAN_POINT ( 'NONE',  ( 11.31249999590322375, -4.235925505221111997, -3.814044456245531567 ) ) ;
#7176 = AXIS2_PLACEMENT_3D ( 'NONE', #4077, #10184, #8672 ) ;
#7177 = AXIS2_PLACEMENT_3D ( 'NONE', #543, #2128, #5029 ) ;
#7178 = CARTESIAN_POINT ( 'NONE',  ( 18.11901729331276911, 5.562305898749055011, 35.00000000000000000 ) ) ;
#7179 = FACE_OUTER_BOUND ( 'NONE', #6409, .T. ) ;
#7180 = ORIENTED_EDGE ( 'NONE', *, *, #2854, .F. ) ;
#7181 = CARTESIAN_POINT ( 'NONE',  ( 7.468749997951615427, 1.510506337161861445, -4.648860486681953397 ) ) ;
#7182 =( NAMED_UNIT ( * ) PLANE_ANGLE_UNIT ( ) SI_UNIT ( $, .RADIAN. ) );
#7183 = DIRECTION ( 'NONE',  ( 1.000000000000000000, 0.000000000000000000, 0.000000000000000000 ) ) ;
#7184 = CARTESIAN_POINT ( 'NONE',  ( 6.500000000000005329, -0.9027913098498965283, 5.699999999999994849 ) ) ;
#7185 = EDGE_LOOP ( 'NONE', ( #19751, #15862, #8968, #798 ) ) ;
#7186 = CARTESIAN_POINT ( 'NONE',  ( -1.310841663519413114, 4.898587196589412829E-16, -4.000000000000000000 ) ) ;
#7187 = EDGE_LOOP ( 'NONE', ( #17805, #6151, #11116, #558, #9557, #422 ) ) ;
#7188 = CARTESIAN_POINT ( 'NONE',  ( 10.46874999795161720, -4.648860486681964055, 1.510506337161829027 ) ) ;
#7189 = DIRECTION ( 'NONE',  ( 0.000000000000000000, 0.000000000000000000, 1.000000000000000000 ) ) ;
#7190 = EDGE_CURVE ( 'NONE', #19316, #18335, #1975, .T. ) ;
#7191 = EDGE_CURVE ( 'NONE', #9505, #19556, #10717, .T. ) ;
#7192 = FACE_OUTER_BOUND ( 'NONE', #7864, .T. ) ;
#7193 = CARTESIAN_POINT ( 'NONE',  ( -1.761396867937200739, 5.421022142882375938, -10.00000000000000533 ) ) ;
#7194 = AXIS2_PLACEMENT_3D ( 'NONE', #17120, #14314, #7901 ) ;
#7195 = VERTEX_POINT ( 'NONE', #18608 ) ;
#7196 = CARTESIAN_POINT ( 'NONE',  ( 2.718131885465892239, 16.91241718341998634, 18.89333555428560274 ) ) ;
#7197 = CARTESIAN_POINT ( 'NONE',  ( -36.00000000000000000, 4.999999999999999112, 2.000000000000000000 ) ) ;
#7198 = ADVANCED_FACE ( 'NONE', ( #1900 ), #6097, .F. ) ;
#7199 = ORIENTED_EDGE ( 'NONE', *, *, #6029, .T. ) ;
#7200 = DIRECTION ( 'NONE',  ( 0.000000000000000000, -1.000000000000000000, 0.000000000000000000 ) ) ;
#7201 = CARTESIAN_POINT ( 'NONE',  ( 5.142044285764733935, -2.620002426024580000, -8.812499995903225525 ) ) ;
#7202 = ORIENTED_EDGE ( 'NONE', *, *, #11176, .F. ) ;
#7203 = CIRCLE ( 'NONE', #16504, 2.524999999999996358 ) ;
#7204 = DIRECTION ( 'NONE',  ( 0.000000000000000000, 0.000000000000000000, -1.000000000000000000 ) ) ;
#7205 = CARTESIAN_POINT ( 'NONE',  ( 2.765633920072238627, 12.59161484032942901, -21.30679549418617924 ) ) ;
#7206 = CARTESIAN_POINT ( 'NONE',  ( -14.86923836996421144, -11.47363181547641275, 32.00000000000000000 ) ) ;
#7207 = VECTOR ( 'NONE', #15790, 1000.000000000000000 ) ;
#7208 = ORIENTED_EDGE ( 'NONE', *, *, #7561, .T. ) ;
#7209 = DIRECTION ( 'NONE',  ( 0.000000000000000000, 0.000000000000000000, 1.000000000000000000 ) ) ;
#7210 = ORIENTED_EDGE ( 'NONE', *, *, #4535, .F. ) ;
#7211 = CARTESIAN_POINT ( 'NONE',  ( 11.32184790671639263, 13.12143529358541016, 32.00000000000000000 ) ) ;
#7212 = ORIENTED_EDGE ( 'NONE', *, *, #15668, .F. ) ;
#7213 = CYLINDRICAL_SURFACE ( 'NONE', #12450, 4.000000000000000000 ) ;
#7214 = DIRECTION ( 'NONE',  ( 0.000000000000000000, 0.000000000000000000, -1.000000000000000000 ) ) ;
#7215 = CARTESIAN_POINT ( 'NONE',  ( 1.749999999999998002, 0.000000000000000000, 0.000000000000000000 ) ) ;
#7216 = CARTESIAN_POINT ( 'NONE',  ( 7.000000000000005329, -5.575441324182703440, 1.185096637661176677 ) ) ;
#7217 = CARTESIAN_POINT ( 'NONE',  ( -20.63749999999999574, 0.000000000000000000, 0.000000000000000000 ) ) ;
#7218 = ORIENTED_EDGE ( 'NONE', *, *, #2362, .T. ) ;
#7219 = TOROIDAL_SURFACE ( 'NONE', #7859, 24.12539914357697768, 8.000000000000000000 ) ;
#7220 = AXIS2_PLACEMENT_3D ( 'NONE', #16212, #11798, #8599 ) ;
#7221 = EDGE_CURVE ( 'NONE', #2723, #11827, #304, .T. ) ;
#7222 = EDGE_CURVE ( 'NONE', #6920, #5362, #12208, .T. ) ;
#7223 = ORIENTED_EDGE ( 'NONE', *, *, #9784, .F. ) ;
#7224 = CARTESIAN_POINT ( 'NONE',  ( -1.899999999999999023, 0.000000000000000000, 0.000000000000000000 ) ) ;
#7225 = CARTESIAN_POINT ( 'NONE',  ( 2.789999999999999147, 22.71065055754452544, 9.836394144775786330 ) ) ;
#7226 = CARTESIAN_POINT ( 'NONE',  ( 8.000000000000000000, 0.000000000000000000, 0.000000000000000000 ) ) ;
#7227 = EDGE_CURVE ( 'NONE', #9218, #10744, #4254, .T. ) ;
#7228 = CARTESIAN_POINT ( 'NONE',  ( -5.000000000000000000, 0.000000000000000000, 37.99999999999999289 ) ) ;
#7229 = ORIENTED_EDGE ( 'NONE', *, *, #5542, .F. ) ;
#7230 = DIRECTION ( 'NONE',  ( 0.000000000000000000, 0.000000000000000000, -1.000000000000000000 ) ) ;
#7231 = VECTOR ( 'NONE', #5262, 1000.000000000000000 ) ;
#7232 = CARTESIAN_POINT ( 'NONE',  ( 0.2590123213420631454, -4.942249507334558700, -7.968749997951616315 ) ) ;
#7233 = CIRCLE ( 'NONE', #2763, 6.735000000000022524 ) ;
#7234 = CARTESIAN_POINT ( 'NONE',  ( 3.814044456245502701, 4.235925505221138643, -11.31249999590322375 ) ) ;
#7235 = ORIENTED_EDGE ( 'NONE', *, *, #6650, .T. ) ;
#7236 = ORIENTED_EDGE ( 'NONE', *, *, #2465, .T. ) ;
#7237 = DIRECTION ( 'NONE',  ( -0.000000000000000000, -0.000000000000000000, 1.000000000000000000 ) ) ;
#7238 = EDGE_CURVE ( 'NONE', #19326, #17134, #6126, .T. ) ;
#7239 = CARTESIAN_POINT ( 'NONE',  ( 14.00000000000000533, -5.668774803599162304, 0.5958122406255995651 ) ) ;
#7240 = ADVANCED_FACE ( 'NONE', ( #10618 ), #3305, .F. ) ;
#7241 = EDGE_LOOP ( 'NONE', ( #6624, #2166, #5955, #14014 ) ) ;
#7242 = CYLINDRICAL_SURFACE ( 'NONE', #12970, 1.000000000000000888 ) ;
#7243 = ORIENTED_EDGE ( 'NONE', *, *, #14483, .F. ) ;
#7244 = FACE_OUTER_BOUND ( 'NONE', #1440, .T. ) ;
#7245 = FACE_OUTER_BOUND ( 'NONE', #4022, .T. ) ;
#7246 = AXIS2_PLACEMENT_3D ( 'NONE', #10537, #5110, #17133 ) ;
#7247 = EDGE_LOOP ( 'NONE', ( #19691, #506, #839, #3872 ) ) ;
#7248 = DIRECTION ( 'NONE',  ( 1.000000000000000000, 0.000000000000000000, 0.000000000000000000 ) ) ;
#7249 = CIRCLE ( 'NONE', #7894, 9.000000000000000000 ) ;
#7250 = DIRECTION ( 'NONE',  ( -1.000000000000000000, -0.000000000000000000, -0.000000000000000000 ) ) ;
#7251 = EDGE_CURVE ( 'NONE', #5965, #8006, #436, .T. ) ;
#7252 = CARTESIAN_POINT ( 'NONE',  ( 6.843749997951615427, 0.000000000000000000, -4.888101187500000222 ) ) ;
#7253 = CYLINDRICAL_SURFACE ( 'NONE', #7455, 2.524999999999995914 ) ;
#7254 = DIRECTION ( 'NONE',  ( 1.000000000000000000, -0.000000000000000000, -0.000000000000000000 ) ) ;
#7255 = FILL_AREA_STYLE ('',( #17993 ) ) ;
#7256 = CARTESIAN_POINT ( 'NONE',  ( 2.765633920072239516, 16.37294372382858398, 18.55949924794898465 ) ) ;
#7257 = EDGE_LOOP ( 'NONE', ( #10426, #10956, #5767, #4744 ) ) ;
#7258 = CARTESIAN_POINT ( 'NONE',  ( 2.789999999999999147, -12.52067188844336165, -20.62201879784926462 ) ) ;
#7259 = AXIS2_PLACEMENT_3D ( 'NONE', #3301, #9607, #15512 ) ;
#7260 = ADVANCED_FACE ( 'NONE', ( #14012 ), #17017, .T. ) ;
#7261 = CARTESIAN_POINT ( 'NONE',  ( 0.000000000000000000, 0.000000000000000000, 32.00000000000000000 ) ) ;
#7262 = CARTESIAN_POINT ( 'NONE',  ( -90.00000000000000000, 0.000000000000000000, 0.000000000000000000 ) ) ;
#7263 = EDGE_CURVE ( 'NONE', #10856, #2723, #7381, .T. ) ;
#7264 = CIRCLE ( 'NONE', #9870, 8.800000000000023803 ) ;
#7265 = CARTESIAN_POINT ( 'NONE',  ( 0.000000000000000000, 0.000000000000000000, 5.700000000000001954 ) ) ;
#7267 = DIRECTION ( 'NONE',  ( 0.000000000000000000, 0.000000000000000000, 1.000000000000000000 ) ) ;
#7266 = B_SPLINE_CURVE_WITH_KNOTS ( 'NONE', 3,
 ( #15955, #2240, #14454, #6829 ),
 .UNSPECIFIED., .F., .F.,
 ( 4, 4 ),
 ( 0.005258110598983623853, 0.005948376585272730464 ),
 .UNSPECIFIED. ) ;
#7268 = VERTEX_POINT ( 'NONE', #14516 ) ;
#7269 = DIRECTION ( 'NONE',  ( 1.000000000000000000, 0.000000000000000000, 0.000000000000000000 ) ) ;
#7270 = CARTESIAN_POINT ( 'NONE',  ( 10.12500000000000178, 0.000000000000000000, 0.000000000000000000 ) ) ;
#7271 = EDGE_LOOP ( 'NONE', ( #13131, #11769 ) ) ;
#7272 = CARTESIAN_POINT ( 'NONE',  ( 10.96874999795161720, 1.773574444220790136, -4.620319390059805187 ) ) ;
#7273 = ADVANCED_FACE ( 'NONE', ( #14210 ), #11501, .F. ) ;
#7274 = CARTESIAN_POINT ( 'NONE',  ( -13.32184790671639618, 13.12143529358541549, 32.00000000000000000 ) ) ;
#7275 = AXIS2_PLACEMENT_3D ( 'NONE', #14771, #1064, #19263 ) ;
#7276 = CARTESIAN_POINT ( 'NONE',  ( 2.718131864678288601, -25.22589920183363432, 2.577209017046923289 ) ) ;
#7277 = CARTESIAN_POINT ( 'NONE',  ( 8.000000000000000000, 0.000000000000000000, 37.99999999999999289 ) ) ;
#7278 = EDGE_CURVE ( 'NONE', #17341, #3605, #9992, .T. ) ;
#7279 = ORIENTED_EDGE ( 'NONE', *, *, #15691, .T. ) ;
#7280 = DIRECTION ( 'NONE',  ( -1.000000000000000000, 0.000000000000000000, -0.000000000000000000 ) ) ;
#7281 = CARTESIAN_POINT ( 'NONE',  ( 1.280903732194421440, -4.780397808154265071, -14.34374999795161543 ) ) ;
#7282 = FILL_AREA_STYLE_COLOUR ( '', #16632 ) ;
#7283 = EDGE_LOOP ( 'NONE', ( #18557, #10303, #9872, #1854, #8912, #18296 ) ) ;
#7284 = LINE ( 'NONE', #13508, #4075 ) ;
#7285 = ORIENTED_EDGE ( 'NONE', *, *, #16385, .F. ) ;
#7286 = CARTESIAN_POINT ( 'NONE',  ( 0.02436607992776368414, 18.55949924794916228, -16.37294372382838148 ) ) ;
#7287 = ADVANCED_FACE ( 'NONE', ( #17308 ), #10014, .T. ) ;
#7288 = CARTESIAN_POINT ( 'NONE',  ( 13.84374999795161543, 3.954556930911862000, 2.873153789725825025 ) ) ;
#7289 = PRODUCT_DEFINITION_SHAPE ( 'NONE', 'NONE',  #19792 ) ;
#7290 = CARTESIAN_POINT ( 'NONE',  ( 7.937500000000000000, 4.582717761692648217, -6.527800000000000047 ) ) ;
#7291 = CIRCLE ( 'NONE', #2508, 4.400000000000000355 ) ;
#7292 = DIRECTION ( 'NONE',  ( -0.000000000000000000, -0.000000000000000000, 1.000000000000000000 ) ) ;
#7293 = ORIENTED_EDGE ( 'NONE', *, *, #9080, .F. ) ;
#7294 = FACE_OUTER_BOUND ( 'NONE', #682, .T. ) ;
#7295 = DIRECTION ( 'NONE',  ( 0.000000000000000000, 0.000000000000000000, 1.000000000000000000 ) ) ;
#7296 = ORIENTED_EDGE ( 'NONE', *, *, #1228, .T. ) ;
#7297 = AXIS2_PLACEMENT_3D ( 'NONE', #17476, #7644, #4259 ) ;
#7298 = CARTESIAN_POINT ( 'NONE',  ( 3.968750000000007994, 6.874076642538976323, 0.000000000000000000 ) ) ;
#7299 = EDGE_CURVE ( 'NONE', #19316, #312, #3042, .T. ) ;
#7300 = DIRECTION ( 'NONE',  ( 1.000000000000000000, 0.000000000000000000, 0.000000000000000000 ) ) ;
#7301 = ORIENTED_EDGE ( 'NONE', *, *, #6398, .T. ) ;
#7302 = CARTESIAN_POINT ( 'NONE',  ( -1.016293382781411125, 4.781284448697194378, -7.468749997951615427 ) ) ;
#7303 = CARTESIAN_POINT ( 'NONE',  ( 11.84374999795161365, 2.444050593749991229, 4.233219804643887585 ) ) ;
#7304 = FACE_BOUND ( 'NONE', #11869, .T. ) ;
#7305 = ORIENTED_EDGE ( 'NONE', *, *, #18592, .T. ) ;
#7306 = CARTESIAN_POINT ( 'NONE',  ( -2.000000000000000888, 8.265000000000021885, 0.000000000000000000 ) ) ;
#7307 = ORIENTED_EDGE ( 'NONE', *, *, #2889, .F. ) ;
#7308 = DIRECTION ( 'NONE',  ( 0.000000000000000000, 0.000000000000000000, 1.000000000000000000 ) ) ;
#7309 = EDGE_LOOP ( 'NONE', ( #19719, #4355, #7924, #6009 ) ) ;
#7310 = AXIS2_PLACEMENT_3D ( 'NONE', #10252, #9871, #15958 ) ;
#7311 =( LENGTH_UNIT ( ) NAMED_UNIT ( * ) SI_UNIT ( .MILLI., .METRE. ) );
#7312 = EDGE_CURVE ( 'NONE', #10781, #10763, #706, .T. ) ;
#7313 = CARTESIAN_POINT ( 'NONE',  ( -11.00000000000000355, 4.898587196589412829E-16, 0.000000000000000000 ) ) ;
#7314 =( BOUNDED_CURVE ( )  B_SPLINE_CURVE ( 2, ( #12791, #8387, #6664, #18059, #12890, #13261, #2079, #18989, #11953, #2279, #14291, #18888, #5281, #11390, #8283 ),
 .UNSPECIFIED., .F., .F. ) 
 B_SPLINE_CURVE_WITH_KNOTS ( ( 3, 2, 2, 2, 2, 2, 2, 3 ),
 ( 0.000000000000000000, 0.04999999999999999584, 0.09999999999999999167, 0.1499999999999999944, 0.1999999999999999833, 0.2500000000000000000, 0.2999999999999999889, 0.3499999999999999778 ),
 .UNSPECIFIED. ) 
 CURVE ( )  GEOMETRIC_REPRESENTATION_ITEM ( )  RATIONAL_B_SPLINE_CURVE ( ( 1.000000000000000000, 0.9876883405951377704, 1.000000000000000000, 0.9876883405951377704, 1.000000000000000000, 0.9876883405951377704, 1.000000000000000000, 0.9876883405951377704, 1.000000000000000000, 0.9876883405951377704, 1.000000000000000000, 0.9876883405951377704, 1.000000000000000000, 0.9876883405951377704, 1.000000000000000000 ) ) 
 REPRESENTATION_ITEM ( '' )  );
#7315 = CARTESIAN_POINT ( 'NONE',  ( 1.510506337161829027, -4.648860486681964055, -10.46874999795161720 ) ) ;
#7316 = CARTESIAN_POINT ( 'NONE',  ( 10.00000000000000533, -4.235925505221111997, -3.814044456245531567 ) ) ;
#7317 = CARTESIAN_POINT ( 'NONE',  ( 2.789999999999999147, -15.74360496233394002, 18.28042085475272671 ) ) ;
#7318 = ORIENTED_EDGE ( 'NONE', *, *, #4413, .T. ) ;
#7319 = CARTESIAN_POINT ( 'NONE',  ( -5.626241948324210540, -16.73597674598852336, -32.00000000000000000 ) ) ;
#7320 = CARTESIAN_POINT ( 'NONE',  ( -25.31088913245573835, 82.80384757729319745, 37.99999999999999289 ) ) ;
#7321 = CIRCLE ( 'NONE', #12782, 0.9999999999999974465 ) ;
#7322 = ORIENTED_EDGE ( 'NONE', *, *, #18492, .T. ) ;
#7323 = CARTESIAN_POINT ( 'NONE',  ( -36.00000000000000000, -5.000000000000001776, -5.000000000000000000 ) ) ;
#7324 = EDGE_CURVE ( 'NONE', #4661, #5399, #18441, .T. ) ;
#7325 = PRODUCT_DEFINITION ( 'UNKNOWN', '', #14993, #6576 ) ;
#7326 = CARTESIAN_POINT ( 'NONE',  ( 2.789999999999999147, 19.91106274590533687, -14.18181402625721077 ) ) ;
#7327 = DIRECTION ( 'NONE',  ( -1.000000000000000000, -0.000000000000000000, -0.000000000000000000 ) ) ;
#7328 = CARTESIAN_POINT ( 'NONE',  ( 13.00000000000000533, -4.611396867937178179, -3.350375938067128967 ) ) ;
#7329 = ORIENTED_EDGE ( 'NONE', *, *, #7705, .F. ) ;
#7330 = CARTESIAN_POINT ( 'NONE',  ( -2.299999999999996270, 1.102182119232620475E-15, 9.000000000000019540 ) ) ;
#7331 = CARTESIAN_POINT ( 'NONE',  ( -2.536997518287239855E-15, -2.975925766232315903E-16, 50.52780000000000626 ) ) ;
#7332 = CARTESIAN_POINT ( 'NONE',  ( -1.280903732194487166, -4.780397808154247308, -8.968749997951611874 ) ) ;
#7333 = FACE_OUTER_BOUND ( 'NONE', #1454, .T. ) ;
#7334 = EDGE_CURVE ( 'NONE', #993, #3395, #17162, .T. ) ;
#7335 = EDGE_LOOP ( 'NONE', ( #17769, #15134, #8661, #6053 ) ) ;
#7336 = ORIENTED_EDGE ( 'NONE', *, *, #16808, .T. ) ;
#7337 = EDGE_CURVE ( 'NONE', #10636, #3405, #8052, .T. ) ;
#7338 = LINE ( 'NONE', #5556, #3460 ) ;
#7339 = VECTOR ( 'NONE', #14077, 1000.000000000000000 ) ;
#7340 = CARTESIAN_POINT ( 'NONE',  ( 9.500000000000003553, -0.3020334839682879413, 5.763142191869155440 ) ) ;
#7341 = CIRCLE ( 'NONE', #7999, 1.000000000000000888 ) ;
#7342 = ORIENTED_EDGE ( 'NONE', *, *, #7337, .T. ) ;
#7343 = CARTESIAN_POINT ( 'NONE',  ( 4.484949146646379781, 3.631840208645794821, -10.50000000000000533 ) ) ;
#7344 = VERTEX_POINT ( 'NONE', #11404 ) ;
#7345 = CYLINDRICAL_SURFACE ( 'NONE', #8379, 1.000000000000003553 ) ;
#7346 = EDGE_CURVE ( 'NONE', #15544, #3222, #8406, .T. ) ;
#7347 = CARTESIAN_POINT ( 'NONE',  ( -17.11901729331276911, 5.562305898749051458, -32.00000000000000000 ) ) ;
#7348 = ORIENTED_EDGE ( 'NONE', *, *, #3982, .T. ) ;
#7349 = AXIS2_PLACEMENT_3D ( 'NONE', #7326, #2937, #2841 ) ;
#7351 = EDGE_CURVE ( 'NONE', #759, #13977, #14779, .T. ) ;
#7350 = ADVANCED_FACE ( 'NONE', ( #17508 ), #1039, .T. ) ;
#7352 = CYLINDRICAL_SURFACE ( 'NONE', #16070, 4.000000000000000000 ) ;
#7353 = CARTESIAN_POINT ( 'NONE',  ( -20.63749999999999929, 4.898587196589412829E-16, 4.000000000000000000 ) ) ;
#7354 = CARTESIAN_POINT ( 'NONE',  ( 3.350375938067065462, -4.611396867937225252, -10.31249999590322552 ) ) ;
#7355 = ORIENTED_EDGE ( 'NONE', *, *, #5636, .F. ) ;
#7356 = FACE_OUTER_BOUND ( 'NONE', #5266, .T. ) ;
#7357 = CARTESIAN_POINT ( 'NONE',  ( -7.841635642041319107E-14, -15.96555658743749717, -18.34439787333524663 ) ) ;
#7358 = ORIENTED_EDGE ( 'NONE', *, *, #18562, .F. ) ;
#7359 = CARTESIAN_POINT ( 'NONE',  ( 0.000000000000000000, 0.000000000000000000, 0.000000000000000000 ) ) ;
#7360 = FACE_BOUND ( 'NONE', #5785, .T. ) ;
#7361 = UNCERTAINTY_MEASURE_WITH_UNIT (LENGTH_MEASURE( 1.000000000000000082E-05 ), #2300, 'distance_accuracy_value', 'NONE');
#7362 = CARTESIAN_POINT ( 'NONE',  ( -4.484949146646330931, 3.631840208645857437, -11.50000000000000355 ) ) ;
#7363 = CARTESIAN_POINT ( 'NONE',  ( 1.039999999999997593, 0.000000000000000000, 0.000000000000000000 ) ) ;
#7364 = CIRCLE ( 'NONE', #16018, 1.000000000000004441 ) ;
#7365 = CARTESIAN_POINT ( 'NONE',  ( -5.207209108562852684, -2.318398865532001363, -9.312499995903225525 ) ) ;
#7366 = ORIENTED_EDGE ( 'NONE', *, *, #19688, .F. ) ;
#7367 = CARTESIAN_POINT ( 'NONE',  ( 2.783025306068355853, -18.43727551351019045, -16.17543236988008815 ) ) ;
#7368 = AXIS2_PLACEMENT_3D ( 'NONE', #6906, #923, #16031 ) ;
#7369 = DIRECTION ( 'NONE',  ( -0.000000000000000000, -1.000000000000000000, -0.000000000000000000 ) ) ;
#7370 = APPLICATION_CONTEXT ( 'automotive_design' ) ;
#7371 = VERTEX_POINT ( 'NONE', #9613 ) ;
#7372 = CARTESIAN_POINT ( 'NONE',  ( 13.84374999795161543, -4.465502636338038123, 1.988169868018562880 ) ) ;
#7373 = CARTESIAN_POINT ( 'NONE',  ( 10.31249999590322552, -5.207209108562803834, -2.318398865532109721 ) ) ;
#7374 = CARTESIAN_POINT ( 'NONE',  ( 2.604434325169353137, -25.77772010606608077, 2.851997810081559503 ) ) ;
#7375 = CARTESIAN_POINT ( 'NONE',  ( -2.000000000000001776, 0.000000000000000000, 0.000000000000000000 ) ) ;
#7376 = ORIENTED_EDGE ( 'NONE', *, *, #18316, .T. ) ;
#7377 = AXIS2_PLACEMENT_3D ( 'NONE', #17150, #14245, #7200 ) ;
#7378 = CIRCLE ( 'NONE', #2291, 8.000000000000000000 ) ;
#7379 = CARTESIAN_POINT ( 'NONE',  ( 11.96874999795161365, 4.888101187500000222, 0.7741991708318884946 ) ) ;
#7380 = DIRECTION ( 'NONE',  ( 0.000000000000000000, 0.000000000000000000, -1.000000000000000000 ) ) ;
#7381 = CIRCLE ( 'NONE', #4222, 1.000000000000004441 ) ;
#7382 = CARTESIAN_POINT ( 'NONE',  ( 1.886022603841227330, 0.000000000000000000, 0.000000000000000000 ) ) ;
#7383 = EDGE_LOOP ( 'NONE', ( #3674, #16892 ) ) ;
#7384 = DIRECTION ( 'NONE',  ( 1.000000000000000000, 0.000000000000000000, 0.000000000000000000 ) ) ;
#7385 = ORIENTED_EDGE ( 'NONE', *, *, #111, .F. ) ;
#7386 = CYLINDRICAL_SURFACE ( 'NONE', #17902, 4.200000000000001066 ) ;
#7387 = CARTESIAN_POINT ( 'NONE',  ( 14.46874999795161720, 2.873153789725825913, 3.954556930911861112 ) ) ;
#7388 = CARTESIAN_POINT ( 'NONE',  ( -3.255998204157480203, -17.85806462366060288, -32.00000000000000000 ) ) ;
#7389 = DIRECTION ( 'NONE',  ( 0.000000000000000000, 1.000000000000000000, 6.982962677686267499E-15 ) ) ;
#7390 = ORIENTED_EDGE ( 'NONE', *, *, #10817, .F. ) ;
#7391 = DIRECTION ( 'NONE',  ( -0.000000000000000000, -0.000000000000000000, 1.000000000000000000 ) ) ;
#7392 = DIRECTION ( 'NONE',  ( 0.000000000000000000, 1.224646799147353947E-16, 1.000000000000000000 ) ) ;
#7393 = AXIS2_PLACEMENT_3D ( 'NONE', #8515, #10116, #16310 ) ;
#7394 = VERTEX_POINT ( 'NONE', #5094 ) ;
#7395 = AXIS2_PLACEMENT_3D ( 'NONE', #2959, #3059, #10968 ) ;
#7396 = AXIS2_PLACEMENT_3D ( 'NONE', #19074, #6757, #3568 ) ;
#7397 = ADVANCED_FACE ( 'NONE', ( #3603 ), #13007, .T. ) ;
#7398 = CIRCLE ( 'NONE', #12548, 1.000000000000002665 ) ;
#7399 = CARTESIAN_POINT ( 'NONE',  ( -3.499494075959816541, 3.499494075959816541, -8.968749997951611874 ) ) ;
#7400 = FACE_OUTER_BOUND ( 'NONE', #11256, .T. ) ;
#7401 = ORIENTED_EDGE ( 'NONE', *, *, #11166, .T. ) ;
#7402 = CARTESIAN_POINT ( 'NONE',  ( 3.846120219227944670, 3.114526743279255161, -11.34374999795161543 ) ) ;
#7403 = CARTESIAN_POINT ( 'NONE',  ( 11.31249999590322375, 4.235925505221138643, 3.814044456245502701 ) ) ;
#7404 = PLANE ( 'NONE',  #2367 ) ;
#7405 = ORIENTED_EDGE ( 'NONE', *, *, #8803, .T. ) ;
#7406 = DIRECTION ( 'NONE',  ( -1.000000000000000000, -0.000000000000000000, 0.000000000000000000 ) ) ;
#7407 = EDGE_LOOP ( 'NONE', ( #1362, #18018, #3327, #7490, #12615, #11532 ) ) ;
#7408 = LINE ( 'NONE', #13533, #15564 ) ;
#7409 = VECTOR ( 'NONE', #19256, 1000.000000000000000 ) ;
#7410 = EDGE_LOOP ( 'NONE', ( #14781, #6682 ) ) ;
#7411 = CARTESIAN_POINT ( 'NONE',  ( 1.545624935189822177E-15, 9.165435523385314198, -6.527800000000000047 ) ) ;
#7412 = CIRCLE ( 'NONE', #5823, 1.000000000000002665 ) ;
#7413 = DIRECTION ( 'NONE',  ( 0.000000000000000000, 0.000000000000000000, 1.000000000000000000 ) ) ;
#7414 = LINE ( 'NONE', #16166, #6654 ) ;
#7415 = CARTESIAN_POINT ( 'NONE',  ( 11.50000000000000355, -2.068159791354146293, -5.387740456496247887 ) ) ;
#7416 = CLOSED_SHELL ( 'NONE', ( #11872, #16151, #15442, #4573, #8849, #1027, #1979, #35, #4639, #7273, #8298, #16705, #42, #19322, #18127, #19345, #5964, #1932, #8432, #14209, #10189, #7607, #19387, #2489, #3531, #5825, #13086, #17674, #16195, #6739, #7157, #14178, #16441, #10720, #12276, #2505, #10483, #15170, #490, #17588, #209, #15926, #17783, #2113, #5401, #4124, #9594, #6006, #6365, #6842, #10145, #12105, #15451, #1952, #1761, #7198, #14608, #4926, #1544, #3382, #6853, #8219, #10323, #12597, #8578, #6638, #5292, #14951, #19227, #18861, #12692, #13936, #3926, #3757, #19617, #7655, #11083, #10281, #19059, #11139, #1276, #9417, #365, #13157, #11292, #8894, #9000, #14784, #18866, #669, #6264, #10737, #3971, #12648, #2440, #5553, #9046, #7088, #2091, #16712, #5168, #8023, #14808, #15707, #18834, #3567, #16556, #17315, #3390, #6452, #15789, #5834, #9514, #16424, #13697, #5379, #18965, #10768 ) ) ;
#7417 = LINE ( 'NONE', #16851, #8865 ) ;
#7418 = EDGE_LOOP ( 'NONE', ( #12926, #2066, #14352, #1050 ) ) ;
#7419 = CIRCLE ( 'NONE', #12566, 7.937500000000000000 ) ;
#7420 = CARTESIAN_POINT ( 'NONE',  ( 2.000000000000001776, 0.000000000000000000, 0.000000000000000000 ) ) ;
#7421 = FACE_OUTER_BOUND ( 'NONE', #7087, .T. ) ;
#7422 = AXIS2_PLACEMENT_3D ( 'NONE', #5940, #8858, #10462 ) ;
#7423 = ORIENTED_EDGE ( 'NONE', *, *, #13212, .T. ) ;
#7424 = ADVANCED_FACE ( 'NONE', ( #12807 ), #5194, .F. ) ;
#7425 = CARTESIAN_POINT ( 'NONE',  ( -3.000000000000002665, 0.000000000000000000, 0.000000000000000000 ) ) ;
#7426 = LINE ( 'NONE', #9153, #7102 ) ;
#7427 = ORIENTED_EDGE ( 'NONE', *, *, #12479, .F. ) ;
#7428 = CARTESIAN_POINT ( 'NONE',  ( 1.800000000000000488, 5.143516556418882928E-16, 4.200000000000000178 ) ) ;
#7429 = CIRCLE ( 'NONE', #1387, 1.199999999999999734 ) ;
#7430 = CARTESIAN_POINT ( 'NONE',  ( 4.484949146646356688, -3.631840208645826351, -11.50000000000000355 ) ) ;
#7431 = AXIS2_PLACEMENT_3D ( 'NONE', #3100, #1602, #7118 ) ;
#7432 = CARTESIAN_POINT ( 'NONE',  ( 0.000000000000000000, 0.000000000000000000, 35.00000000000000000 ) ) ;
#7433 = ORIENTED_EDGE ( 'NONE', *, *, #3875, .T. ) ;
#7434 = DIRECTION ( 'NONE',  ( 1.000000000000000000, 0.000000000000000000, 0.000000000000000000 ) ) ;
#7435 = ORIENTED_EDGE ( 'NONE', *, *, #14270, .F. ) ;
#7436 = CARTESIAN_POINT ( 'NONE',  ( 0.000000000000000000, 0.000000000000000000, 0.000000000000000000 ) ) ;
#7437 = CARTESIAN_POINT ( 'NONE',  ( 2.444050593749960587, -4.233219804643904460, -6.468749997951615427 ) ) ;
#7438 = CARTESIAN_POINT ( 'NONE',  ( 1.185096637661176677, -5.575441324182703440, -8.312499995903225525 ) ) ;
#7439 = ORIENTED_EDGE ( 'NONE', *, *, #13766, .T. ) ;
#7440 = ORIENTED_EDGE ( 'NONE', *, *, #7238, .T. ) ;
#7441 = DIRECTION ( 'NONE',  ( 0.000000000000000000, 0.000000000000000000, -1.000000000000000000 ) ) ;
#7442 = CARTESIAN_POINT ( 'NONE',  ( 5.387740456496232788, 2.068159791354184485, -12.81249999590322552 ) ) ;
#7443 = ORIENTED_EDGE ( 'NONE', *, *, #4043, .T. ) ;
#7444 = ADVANCED_FACE ( 'NONE', ( #19288 ), #13199, .F. ) ;
#7445 = EDGE_CURVE ( 'NONE', #2779, #1853, #10202, .T. ) ;
#7446 = DIRECTION ( 'NONE',  ( 1.000000000000000000, 0.000000000000000000, 0.000000000000000000 ) ) ;
#7447 = ORIENTED_EDGE ( 'NONE', *, *, #17815, .T. ) ;
#7448 = DIRECTION ( 'NONE',  ( 0.000000000000000000, 0.000000000000000000, 1.000000000000000000 ) ) ;
#7449 = AXIS2_PLACEMENT_3D ( 'NONE', #13301, #19112, #19017 ) ;
#7450 = CARTESIAN_POINT ( 'NONE',  ( 0.02436607992775978102, -12.59161484032896361, -21.30679549418645280 ) ) ;
#7451 = EDGE_CURVE ( 'NONE', #4088, #8718, #13321, .T. ) ;
#7452 = ORIENTED_EDGE ( 'NONE', *, *, #12892, .F. ) ;
#7453 = ADVANCED_FACE ( 'NONE', ( #10105 ), #19485, .T. ) ;
#7454 = PRESENTATION_LAYER_ASSIGNMENT (  '', '', ( #1091 ) ) ;
#7455 = AXIS2_PLACEMENT_3D ( 'NONE', #15993, #14692, #978 ) ;
#7456 = CARTESIAN_POINT ( 'NONE',  ( -5.207209108562804722, 2.318398865532109276, -15.31249999590322552 ) ) ;
#7457 = CARTESIAN_POINT ( 'NONE',  ( 1.039999999999996039, 24.89775460606832169, 12.96210679857795256 ) ) ;
#7458 = CARTESIAN_POINT ( 'NONE',  ( 4.080749450109622423, -4.080749450109678378, -9.812499995903225525 ) ) ;
#7459 = ORIENTED_EDGE ( 'NONE', *, *, #15502, .F. ) ;
#7460 = DIRECTION ( 'NONE',  ( 0.000000000000000000, 0.000000000000000000, 1.000000000000000000 ) ) ;
#7461 =( NAMED_UNIT ( * ) SI_UNIT ( $, .STERADIAN. ) SOLID_ANGLE_UNIT ( ) );
#7462 = LINE ( 'NONE', #10393, #5487 ) ;
#7463 = VECTOR ( 'NONE', #12796, 1000.000000000000000 ) ;
#7464 = VERTEX_POINT ( 'NONE', #5773 ) ;
#7465 = EDGE_CURVE ( 'NONE', #16071, #7096, #17372, .T. ) ;
#7466 = CARTESIAN_POINT ( 'NONE',  ( -19.00000000000000355, 3.278623949159157558, -2.625000000000002220 ) ) ;
#7467 = CYLINDRICAL_SURFACE ( 'NONE', #4374, 13.19999999999999929 ) ;
#7468 = CARTESIAN_POINT ( 'NONE',  ( -4.936344801571268093, 2.850000000000057820, -11.00000000000000711 ) ) ;
#7469 = DIRECTION ( 'NONE',  ( -0.7071067811865492381, 0.000000000000000000, 0.7071067811865457964 ) ) ;
#7470 = PRODUCT_DEFINITION ( 'UNKNOWN', '', #4760, #16000 ) ;
#7471 = AXIS2_PLACEMENT_3D ( 'NONE', #17990, #19576, #16586 ) ;
#7472 = CARTESIAN_POINT ( 'NONE',  ( 3.954556930911861112, 2.873153789725825913, -14.84374999795161543 ) ) ;
#7473 = ADVANCED_FACE ( 'NONE', ( #13388 ), #5877, .T. ) ;
#7474 = ORIENTED_EDGE ( 'NONE', *, *, #5090, .F. ) ;
#7475 = CARTESIAN_POINT ( 'NONE',  ( -16.19790265903627713, 9.644882309621941374, 32.00000000000000000 ) ) ;
#7476 = CARTESIAN_POINT ( 'NONE',  ( -3.846120219227901149, 3.114526743279308896, -11.96874999795161365 ) ) ;
#7477 = ORIENTED_EDGE ( 'NONE', *, *, #879, .T. ) ;
#7478 = CARTESIAN_POINT ( 'NONE',  ( -17.28688694438836393, -7.664027248171298545, -32.00000000000000000 ) ) ;
#7479 = AXIS2_PLACEMENT_3D ( 'NONE', #11612, #17814, #14530 ) ;
#7480 = EDGE_CURVE ( 'NONE', #16413, #17840, #19388, .T. ) ;
#7481 = CARTESIAN_POINT ( 'NONE',  ( -5.700000000000000178, -2.180340287075187351E-16, -13.97977757194593273 ) ) ;
#7482 = CARTESIAN_POINT ( 'NONE',  ( 0.5279273381794611364, 3.461047254864636713, -26.82026385750174668 ) ) ;
#7483 = CARTESIAN_POINT ( 'NONE',  ( 9.500000000000005329, 4.840010801796481132, 3.143139765844623401 ) ) ;
#7484 = ORIENTED_EDGE ( 'NONE', *, *, #10697, .F. ) ;
#7485 = VECTOR ( 'NONE', #19107, 1000.000000000000000 ) ;
#7486 = CARTESIAN_POINT ( 'NONE',  ( 14.19790265903627180, 9.644882309621939598, 32.00000000000000000 ) ) ;
#7487 = SHAPE_REPRESENTATION_RELATIONSHIP ( 'NONE' , 'NONE' ,  #11438, #8048 ) ;
#7488 = DIRECTION ( 'NONE',  ( -0.000000000000000000, -0.000000000000000000, -1.000000000000000000 ) ) ;
#7489 = EDGE_CURVE ( 'NONE', #10072, #12340, #12227, .T. ) ;
#7490 = ORIENTED_EDGE ( 'NONE', *, *, #12482, .F. ) ;
#7491 = DIRECTION ( 'NONE',  ( -0.000000000000000000, -0.000000000000000000, 1.000000000000000000 ) ) ;
#7492 = CARTESIAN_POINT ( 'NONE',  ( 9.468749997951615427, 0.5109457054261445919, 4.861323657744411442 ) ) ;
#7493 = CARTESIAN_POINT ( 'NONE',  ( 11.46874999795161543, -4.888101187500000222, -3.383411828340740850E-14 ) ) ;
#7494 = CARTESIAN_POINT ( 'NONE',  ( 7.468749997951615427, 1.510506337161861445, -4.648860486681953397 ) ) ;
#7495 = DIRECTION ( 'NONE',  ( 1.000000000000000000, 0.000000000000000000, 0.000000000000000000 ) ) ;
#7496 = ADVANCED_FACE ( 'NONE', ( #11994 ), #16298, .T. ) ;
#7497 = CARTESIAN_POINT ( 'NONE',  ( 1.280903732194454081, 4.780397808154257078, -9.343749997951615427 ) ) ;
#7498 = EDGE_CURVE ( 'NONE', #17369, #5524, #684, .T. ) ;
#7499 = ORIENTED_EDGE ( 'NONE', *, *, #6737, .T. ) ;
#7500 = CARTESIAN_POINT ( 'NONE',  ( 17.96448111170888851, 1.130229351527639148, -35.00000000000000000 ) ) ;
#7501 = CARTESIAN_POINT ( 'NONE',  ( 18.68117051311639543, -3.372863662543048591, -32.00000000000000000 ) ) ;
#7502 = AXIS2_PLACEMENT_3D ( 'NONE', #14084, #9202, #18490 ) ;
#7503 = EDGE_LOOP ( 'NONE', ( #16156, #5057, #3968, #1677 ) ) ;
#7504 = DIRECTION ( 'NONE',  ( -1.000000000000000000, -0.000000000000000000, -0.000000000000000000 ) ) ;
#7505 = LINE ( 'NONE', #6205, #1820 ) ;
#7506 = EDGE_LOOP ( 'NONE', ( #18358, #4666 ) ) ;
#7507 = CARTESIAN_POINT ( 'NONE',  ( -7.765813458258934317E-14, -24.22524813288764278, 2.133839912090720325 ) ) ;
#7508 = CARTESIAN_POINT ( 'NONE',  ( 14.81249999590322552, -1.493657965219523209, 5.574407415329156734 ) ) ;
#7509 = CARTESIAN_POINT ( 'NONE',  ( -4.648860486681953397, 1.510506337161861445, -7.468749997951615427 ) ) ;
#7510 = EDGE_CURVE ( 'NONE', #201, #2502, #7167, .T. ) ;
#7511 = ORIENTED_EDGE ( 'NONE', *, *, #4434, .T. ) ;
#7512 = DIRECTION ( 'NONE',  ( -1.000000000000000000, 0.000000000000000000, 0.000000000000000000 ) ) ;
#7513 = VERTEX_POINT ( 'NONE', #4584 ) ;
#7514 = DIRECTION ( 'NONE',  ( -0.000000000000000000, -0.000000000000000000, 1.000000000000000000 ) ) ;
#7515 = ORIENTED_EDGE ( 'NONE', *, *, #5946, .F. ) ;
#7516 = CARTESIAN_POINT ( 'NONE',  ( 0.02436607992776411782, 22.71065055754465689, -9.836394144775473691 ) ) ;
#7517 = CIRCLE ( 'NONE', #11049, 0.1999999999999996503 ) ;
#7518 = DIRECTION ( 'NONE',  ( 0.000000000000000000, 0.000000000000000000, -1.000000000000000000 ) ) ;
#7519 = CARTESIAN_POINT ( 'NONE',  ( 1.949486339718610296E-19, -22.37986894186666831, -9.514945144208986960 ) ) ;
#7520 = CARTESIAN_POINT ( 'NONE',  ( 14.00000000000000533, 2.318398865532109276, -5.207209108562804722 ) ) ;
#7521 = CARTESIAN_POINT ( 'NONE',  ( 1.749999999999998002, 20.02152543075374069, -19.67366047555509212 ) ) ;
#7522 = EDGE_CURVE ( 'NONE', #6004, #10056, #9679, .T. ) ;
#7523 = ORIENTED_EDGE ( 'NONE', *, *, #12236, .F. ) ;
#7524 = DIRECTION ( 'NONE',  ( 0.000000000000000000, 0.000000000000000000, 1.000000000000000000 ) ) ;
#7525 = SURFACE_STYLE_USAGE ( .BOTH. , #9047 ) ;
#7526 = CONICAL_SURFACE ( 'NONE', #533, 4.000000000000000000, 0.2132412839022289897 ) ;
#7527 = ORIENTED_EDGE ( 'NONE', *, *, #18445, .F. ) ;
#7528 = EDGE_CURVE ( 'NONE', #18696, #6248, #16697, .T. ) ;
#7529 = AXIS2_PLACEMENT_3D ( 'NONE', #8720, #10046, #11531 ) ;
#7530 = DIRECTION ( 'NONE',  ( -1.000000000000000000, -0.000000000000000000, -0.000000000000000000 ) ) ;
#7531 = CARTESIAN_POINT ( 'NONE',  ( 16.19790265903627358, 9.644882309621939598, 32.00000000000000000 ) ) ;
#7532 = EDGE_LOOP ( 'NONE', ( #17572, #13360, #2753, #9335 ) ) ;
#7533 = CARTESIAN_POINT ( 'NONE',  ( -11.58013454126452579, -14.56230589874905235, 32.00000000000000000 ) ) ;
#7534 = CARTESIAN_POINT ( 'NONE',  ( 3.631840208645826795, 4.484949146646356688, -6.500000000000005329 ) ) ;
#7535 = CARTESIAN_POINT ( 'NONE',  ( 1.799999999999999600, 0.000000000000000000, 0.000000000000000000 ) ) ;
#7536 = VERTEX_POINT ( 'NONE', #19779 ) ;
#7537 = CARTESIAN_POINT ( 'NONE',  ( 4.233219804643887585, 2.444050593749990785, -11.46874999795161543 ) ) ;
#7538 = ORIENTED_EDGE ( 'NONE', *, *, #1846, .T. ) ;
#7539 = DIRECTION ( 'NONE',  ( -0.9966499414291889458, -0.08178566041302280654, -1.075658682394499197E-16 ) ) ;
#7540 = CARTESIAN_POINT ( 'NONE',  ( 2.257825459230522913, -4.993157874727630841, -26.58873630738057159 ) ) ;
#7541 = FILL_AREA_STYLE_COLOUR ( '', #16929 ) ;
#7542 = ORIENTED_EDGE ( 'NONE', *, *, #6295, .T. ) ;
#7543 = ORIENTED_EDGE ( 'NONE', *, *, #1885, .T. ) ;
#7544 = CARTESIAN_POINT ( 'NONE',  ( 2.000000000000000000, 1.999999999999998224, 41.99999999999999289 ) ) ;
#7545 = TOROIDAL_SURFACE ( 'NONE', #1492, 24.12539914357697413, 8.000000000000000000 ) ;
#7546 = CARTESIAN_POINT ( 'NONE',  ( 5.207209108562820710, -2.318398865532073305, -15.31249999590322552 ) ) ;
#7547 = EDGE_CURVE ( 'NONE', #13907, #16740, #4683, .T. ) ;
#7548 = CIRCLE ( 'NONE', #5320, 1.000000000000000888 ) ;
#7549 = ORIENTED_EDGE ( 'NONE', *, *, #17414, .T. ) ;
#7550 = DIRECTION ( 'NONE',  ( 0.000000000000000000, 0.000000000000000000, 1.000000000000000000 ) ) ;
#7551 = EDGE_LOOP ( 'NONE', ( #11446, #11108, #10416, #5652 ) ) ;
#7552 = DIRECTION ( 'NONE',  ( -0.000000000000000000, -0.000000000000000000, 1.000000000000000000 ) ) ;
#7553 = ORIENTED_EDGE ( 'NONE', *, *, #16459, .T. ) ;
#7554 =( BOUNDED_CURVE ( )  B_SPLINE_CURVE ( 2, ( #2461, #4074, #14687, #3776, #19272, #15890, #2275, #14591, #10182, #14390, #13081, #8574, #12887, #18983, #19079 ),
 .UNSPECIFIED., .F., .F. ) 
 B_SPLINE_CURVE_WITH_KNOTS ( ( 3, 2, 2, 2, 2, 2, 2, 3 ),
 ( 0.000000000000000000, 0.05000000000000000278, 0.1000000000000000056, 0.1499999999999999944, 0.2000000000000000111, 0.2500000000000000000, 0.2999999999999999889, 0.3078686208676164604 ),
 .UNSPECIFIED. ) 
 CURVE ( )  GEOMETRIC_REPRESENTATION_ITEM ( )  RATIONAL_B_SPLINE_CURVE ( ( 1.000000000000000000, 0.9876883405951377704, 1.000000000000000000, 0.9876883405951377704, 1.000000000000000000, 0.9876883405951377704, 1.000000000000000000, 0.9876883405951377704, 1.000000000000000000, 0.9876883405951377704, 1.000000000000000000, 0.9876883405951377704, 1.000000000000000000, 0.9980624843978382899, 0.9967347918236166837 ) ) 
 REPRESENTATION_ITEM ( '' )  );
#7555 = VECTOR ( 'NONE', #6257, 1000.000000000000000 ) ;
#7556 = EDGE_CURVE ( 'NONE', #11278, #5399, #3297, .T. ) ;
#7557 = VECTOR ( 'NONE', #11989, 1000.000000000000000 ) ;
#7558 = DIRECTION ( 'NONE',  ( 1.000000000000000000, 0.000000000000000000, 0.000000000000000000 ) ) ;
#7559 = CARTESIAN_POINT ( 'NONE',  ( 7.843749997951614539, 1.510506337161861445, -4.648860486681953397 ) ) ;
#7560 = EDGE_CURVE ( 'NONE', #18392, #530, #7572, .T. ) ;
#7561 = EDGE_CURVE ( 'NONE', #12604, #17114, #10787, .T. ) ;
#7562 = FACE_OUTER_BOUND ( 'NONE', #1135, .T. ) ;
#7563 = ORIENTED_EDGE ( 'NONE', *, *, #11668, .T. ) ;
#7564 = DIRECTION ( 'NONE',  ( 1.000000000000000000, 0.000000000000000000, -0.000000000000000000 ) ) ;
#7565 = CARTESIAN_POINT ( 'NONE',  ( 2.790000000000000480, 15.96500990068124715, 18.34424029220116736 ) ) ;
#7566 = ORIENTED_EDGE ( 'NONE', *, *, #4028, .F. ) ;
#7567 = CARTESIAN_POINT ( 'NONE',  ( -9.000000000000000000, 0.000000000000000000, -35.00000000000000000 ) ) ;
#7568 = DIRECTION ( 'NONE',  ( -1.000000000000000000, 0.000000000000000000, -0.000000000000000000 ) ) ;
#7569 = DIRECTION ( 'NONE',  ( 0.000000000000000000, 0.000000000000000000, -1.000000000000000000 ) ) ;
#7570 = EDGE_CURVE ( 'NONE', #13799, #4257, #5184, .T. ) ;
#7571 = EDGE_CURVE ( 'NONE', #4614, #16516, #14460, .T. ) ;
#7572 = LINE ( 'NONE', #10692, #17011 ) ;
#7573 = AXIS2_PLACEMENT_3D ( 'NONE', #9841, #2314, #17624 ) ;
#7574 = CARTESIAN_POINT ( 'NONE',  ( 12.99999999999999467, 4.390212428369212105, 2.150226904532439143 ) ) ;
#7575 = CIRCLE ( 'NONE', #10158, 1.000000000000004441 ) ;
#7576 = EDGE_LOOP ( 'NONE', ( #14764, #7875 ) ) ;
#7577 = DIRECTION ( 'NONE',  ( 0.000000000000000000, 0.000000000000000000, -1.000000000000000000 ) ) ;
#7578 = CARTESIAN_POINT ( 'NONE',  ( 2.783068945535914551, -24.42321038836784197, 2.248820353272884542 ) ) ;
#7579 = ORIENTED_EDGE ( 'NONE', *, *, #1143, .T. ) ;
#7580 = CARTESIAN_POINT ( 'NONE',  ( 12.81249999590322552, -3.631840208645826351, 4.484949146646356688 ) ) ;
#7581 = CARTESIAN_POINT ( 'NONE',  ( 13.81249999590322552, -0.3020334839682081163, -5.763142191869158992 ) ) ;
#7582 = DIRECTION ( 'NONE',  ( 1.000000000000000000, 0.000000000000000000, 0.000000000000000000 ) ) ;
#7583 = CARTESIAN_POINT ( 'NONE',  ( 1.039999999999995595, 20.02152543075345648, 19.67366047555537278 ) ) ;
#7584 = PRODUCT_RELATED_PRODUCT_CATEGORY ( 'part', '', ( #17533 ) ) ;
#7585 = VERTEX_POINT ( 'NONE', #13986 ) ;
#7586 = AXIS2_PLACEMENT_3D ( 'NONE', #8684, #16496, #14794 ) ;
#7587 = CARTESIAN_POINT ( 'NONE',  ( 12.96874999795161543, 4.409619785863906571, 2.246813503491833508 ) ) ;
#7588 =( NAMED_UNIT ( * ) SI_UNIT ( $, .STERADIAN. ) SOLID_ANGLE_UNIT ( ) );
#7589 = DIRECTION ( 'NONE',  ( 0.000000000000000000, 0.000000000000000000, 1.000000000000000000 ) ) ;
#7590 = AXIS2_PLACEMENT_3D ( 'NONE', #9016, #1416, #5998 ) ;
#7591 =( LENGTH_UNIT ( ) NAMED_UNIT ( * ) SI_UNIT ( .MILLI., .METRE. ) );
#7592 = VERTEX_POINT ( 'NONE', #16803 ) ;
#7593 = DIRECTION ( 'NONE',  ( 1.000000000000000000, 6.419766481290786633E-33, -0.000000000000000000 ) ) ;
#7594 = CARTESIAN_POINT ( 'NONE',  ( -39.64101615137763446, 12.80384757729311573, 41.99999999999999289 ) ) ;
#7595 = DIRECTION ( 'NONE',  ( -1.000000000000000000, 0.000000000000000000, 0.000000000000000000 ) ) ;
#7596 = EDGE_CURVE ( 'NONE', #18721, #9320, #1990, .T. ) ;
#7597 = CARTESIAN_POINT ( 'NONE',  ( 8.343749997951611874, 2.246813503491833508, -4.409619785863906571 ) ) ;
#7598 = ORIENTED_EDGE ( 'NONE', *, *, #1019, .T. ) ;
#7599 = EDGE_CURVE ( 'NONE', #8384, #13729, #12544, .T. ) ;
#7600 = DIRECTION ( 'NONE',  ( -0.000000000000000000, -0.000000000000000000, 1.000000000000000000 ) ) ;
#7601 = CARTESIAN_POINT ( 'NONE',  ( 2.765633920072238627, 5.391175441198956086, -24.15498966839956907 ) ) ;
#7602 = ORIENTED_EDGE ( 'NONE', *, *, #816, .T. ) ;
#7603 = DIRECTION ( 'NONE',  ( 0.000000000000000000, 0.000000000000000000, -1.000000000000000000 ) ) ;
#7604 = CARTESIAN_POINT ( 'NONE',  ( 7.626241948324204323, -16.73597674598852691, -32.00000000000000000 ) ) ;
#7605 = AXIS2_PLACEMENT_3D ( 'NONE', #2167, #12978, #17677 ) ;
#7606 = ORIENTED_EDGE ( 'NONE', *, *, #111, .T. ) ;
#7607 = ADVANCED_FACE ( 'NONE', ( #9191 ), #13786, .F. ) ;
#7608 = B_SPLINE_CURVE_WITH_KNOTS ( 'NONE', 3,
 ( #17334, #3625, #12736, #9944, #3821, #5117 ),
 .UNSPECIFIED., .F., .F.,
 ( 4, 2, 4 ),
 ( 4.462636793130641501E-07, 0.001879885123570645879, 0.003759323983461978699 ),
 .UNSPECIFIED. ) ;
#7609 = CARTESIAN_POINT ( 'NONE',  ( -1.510506337161861667, 4.648860486681953397, -10.46874999795161720 ) ) ;
#7610 = DIRECTION ( 'NONE',  ( 1.000000000000000000, 0.000000000000000000, 0.000000000000000000 ) ) ;
#7611 = ORIENTED_EDGE ( 'NONE', *, *, #9703, .F. ) ;
#7612 = CARTESIAN_POINT ( 'NONE',  ( 12.81249999590322552, 2.068159791354184485, 5.387740456496232788 ) ) ;
#7613 = EDGE_CURVE ( 'NONE', #5363, #1292, #4964, .T. ) ;
#7614 = DIRECTION ( 'NONE',  ( 0.000000000000000000, 0.000000000000000000, 1.000000000000000000 ) ) ;
#7615 = ORIENTED_EDGE ( 'NONE', *, *, #4623, .F. ) ;
#7616 = CARTESIAN_POINT ( 'NONE',  ( 2.789999999999999147, -7.334849878007332791, -23.31896751603339979 ) ) ;
#7617 = ORIENTED_EDGE ( 'NONE', *, *, #13847, .T. ) ;
#7619 = DIRECTION ( 'NONE',  ( -1.000000000000000000, 6.982962677686267499E-15, 0.000000000000000000 ) ) ;
#7618 = VECTOR ( 'NONE', #9142, 1000.000000000000227 ) ;
#7620 = EDGE_LOOP ( 'NONE', ( #13782, #9777, #10149, #6335 ) ) ;
#7621 = CARTESIAN_POINT ( 'NONE',  ( -11.00000000000000355, 4.215373648918917304, -3.375000000000002665 ) ) ;
#7622 = CARTESIAN_POINT ( 'NONE',  ( 0.000000000000000000, 0.000000000000000000, -6.502399999999998847 ) ) ;
#7623 = DIRECTION ( 'NONE',  ( 0.000000000000000000, 0.000000000000000000, 1.000000000000000000 ) ) ;
#7624 = DIRECTION ( 'NONE',  ( -1.000000000000000000, 0.000000000000000000, -0.000000000000000000 ) ) ;
#7625 = CARTESIAN_POINT ( 'NONE',  ( 13.00000000000000000, 0.2705398332808751638, 4.881009025374877908 ) ) ;
#7626 = PRODUCT_DEFINITION_FORMATION_WITH_SPECIFIED_SOURCE ( 'ANY', '', #9709, .NOT_KNOWN. ) ;
#7627 = VERTEX_POINT ( 'NONE', #3276 ) ;
#7628 = DIRECTION ( 'NONE',  ( -0.000000000000000000, -0.000000000000000000, 1.000000000000000000 ) ) ;
#7629 = B_SPLINE_CURVE_WITH_KNOTS ( 'NONE', 1,
 ( #1978, #7976 ),
 .UNSPECIFIED., .F., .F.,
 ( 2, 2 ),
 ( 0.000000000000000000, 1.000000000000000000 ),
 .UNSPECIFIED. ) ;
#7630 = B_SPLINE_CURVE_WITH_KNOTS ( 'NONE', 1,
 ( #1022, #2517 ),
 .UNSPECIFIED., .F., .F.,
 ( 2, 2 ),
 ( 0.000000000000000000, 1.000000000000000000 ),
 .UNSPECIFIED. ) ;
#7631 = CARTESIAN_POINT ( 'NONE',  ( -2.000000000000001776, -3.950217066951267952, 3.681818181818181213 ) ) ;
#7632 = EDGE_CURVE ( 'NONE', #16071, #14651, #17089, .T. ) ;
#7633 = VERTEX_POINT ( 'NONE', #9392 ) ;
#7634 = CARTESIAN_POINT ( 'NONE',  ( 2.030753605846574494, 3.797885586973597682, -27.31305418910206129 ) ) ;
#7635 = CARTESIAN_POINT ( 'NONE',  ( 15.28688694438835505, -7.664027248171309203, -35.00000000000000000 ) ) ;
#7636 = ORIENTED_EDGE ( 'NONE', *, *, #7174, .T. ) ;
#7638 = CIRCLE ( 'NONE', #18832, 5.700000000000001954 ) ;
#7637 = CARTESIAN_POINT ( 'NONE',  ( 2.789999999999999147, 22.25075486061751207, -9.324097380959219805 ) ) ;
#7639 = CARTESIAN_POINT ( 'NONE',  ( 5.207209108562838473, 2.318398865532038666, -8.000000000000005329 ) ) ;
#7640 = SURFACE_STYLE_USAGE ( .BOTH. , #15361 ) ;
#7641 = ORIENTED_EDGE ( 'NONE', *, *, #8935, .F. ) ;
#7642 = LINE ( 'NONE', #13757, #12611 ) ;
#7643 = ORIENTED_EDGE ( 'NONE', *, *, #17514, .T. ) ;
#7644 = DIRECTION ( 'NONE',  ( 0.000000000000000000, 0.000000000000000000, 1.000000000000000000 ) ) ;
#7645 = DIRECTION ( 'NONE',  ( -1.000000000000000000, -0.000000000000000000, -0.000000000000000000 ) ) ;
#7646 = SURFACE_STYLE_USAGE ( .BOTH. , #6044 ) ;
#7647 = ORIENTED_EDGE ( 'NONE', *, *, #4310, .F. ) ;
#7648 = ORIENTED_EDGE ( 'NONE', *, *, #9847, .T. ) ;
#7649 = CARTESIAN_POINT ( 'NONE',  ( 1.394999999999998685, 27.68468304288265358, -4.633866840648637186 ) ) ;
#7650 = DIRECTION ( 'NONE',  ( -1.000000000000000000, -0.000000000000000000, -0.000000000000000000 ) ) ;
#7651 = EDGE_LOOP ( 'NONE', ( #3467, #13166, #9459, #15462, #85, #12955, #14346, #14023, #4167, #8073 ) ) ;
#7652 = ORIENTED_EDGE ( 'NONE', *, *, #12307, .F. ) ;
#7653 = CARTESIAN_POINT ( 'NONE',  ( -1.000000000000001998, 18.00000000000000355, 32.00000000000000000 ) ) ;
#7654 = VERTEX_POINT ( 'NONE', #3178 ) ;
#7655 = ADVANCED_FACE ( 'NONE', ( #9288 ), #15391, .F. ) ;
#7656 = DIRECTION ( 'NONE',  ( 0.000000000000000000, -0.5000000000000098810, 0.8660254037844330455 ) ) ;
#7657 = CARTESIAN_POINT ( 'NONE',  ( -9.671566133830877376, 15.77352024078954429, -32.00000000000000000 ) ) ;
#7658 = LINE ( 'NONE', #1275, #18348 ) ;
#7659 = ORIENTED_EDGE ( 'NONE', *, *, #4982, .T. ) ;
#7660 = AXIS2_PLACEMENT_3D ( 'NONE', #7868, #15586, #3274 ) ;
#7661 = ORIENTED_EDGE ( 'NONE', *, *, #6949, .F. ) ;
#7663 = CARTESIAN_POINT ( 'NONE',  ( 0.1855655959470664251, -17.45907811351468553, 19.17825124759772493 ) ) ;
#7662 = B_SPLINE_CURVE_WITH_KNOTS ( 'NONE', 3,
 ( #17869, #7946, #1463, #55, #10862, #255 ),
 .UNSPECIFIED., .F., .F.,
 ( 4, 2, 4 ),
 ( 4.462636808949230078E-07, 0.001879885123572232067, 0.003759323983463569441 ),
 .UNSPECIFIED. ) ;
#7664 =( LENGTH_UNIT ( ) NAMED_UNIT ( * ) SI_UNIT ( .MILLI., .METRE. ) );
#7665 = DIRECTION ( 'NONE',  ( 1.000000000000000000, 0.000000000000000000, 0.000000000000000000 ) ) ;
#7666 = ORIENTED_EDGE ( 'NONE', *, *, #2536, .F. ) ;
#7667 = DIRECTION ( 'NONE',  ( 0.000000000000000000, 6.870191984066573782E-16, -1.000000000000000000 ) ) ;
#7668 = CARTESIAN_POINT ( 'NONE',  ( 0.000000000000000000, 0.000000000000000000, -35.00000000000000000 ) ) ;
#7669 = DIRECTION ( 'NONE',  ( 1.000000000000000000, 6.419766481290786633E-33, -0.000000000000000000 ) ) ;
#7670 = CARTESIAN_POINT ( 'NONE',  ( 0.000000000000000000, 0.000000000000000000, 29.00000000000000355 ) ) ;
#7671 = B_SPLINE_CURVE_WITH_KNOTS ( 'NONE', 3,
 ( #18179, #12074, #1069, #4166, #10380, #1168 ),
 .UNSPECIFIED., .F., .F.,
 ( 4, 2, 4 ),
 ( 1.979325885420574018E-07, 0.001878588715165606469, 0.003756979497742670565 ),
 .UNSPECIFIED. ) ;
#7672 = CARTESIAN_POINT ( 'NONE',  ( 0.000000000000000000, -12.52067188844364587, 20.62201879784910119 ) ) ;
#7673 = EDGE_LOOP ( 'NONE', ( #19372, #10560, #4575, #13926 ) ) ;
#7674 = CARTESIAN_POINT ( 'NONE',  ( 2.500000000000002220, 8.013782491920515573E-16, -6.543750000000017941 ) ) ;
#7675 = EDGE_CURVE ( 'NONE', #11508, #9467, #5808, .T. ) ;
#7676 =( BOUNDED_CURVE ( )  B_SPLINE_CURVE ( 2, ( #1025, #14836, #5616, #1130, #13421, #19521, #386, #3683, #5082 ),
 .UNSPECIFIED., .F., .F. ) 
 B_SPLINE_CURVE_WITH_KNOTS ( ( 3, 2, 2, 2, 3 ),
 ( 0.000000000000000000, 0.04999999999999999584, 0.09999999999999999167, 0.1499999999999999944, 0.1666819079834116757 ),
 .UNSPECIFIED. ) 
 CURVE ( )  GEOMETRIC_REPRESENTATION_ITEM ( )  RATIONAL_B_SPLINE_CURVE ( ( 1.000000000000000000, 0.9876883405951377704, 1.000000000000000000, 0.9876883405951377704, 1.000000000000000000, 0.9876883405951377704, 1.000000000000000000, 0.9958923606136996787, 0.9945256517182512468 ) ) 
 REPRESENTATION_ITEM ( '' )  );
#7677 = DIRECTION ( 'NONE',  ( 0.000000000000000000, 0.000000000000000000, -1.000000000000000000 ) ) ;
#7678 = AXIS2_PLACEMENT_3D ( 'NONE', #5402, #13109, #906 ) ;
#7679 = ORIENTED_EDGE ( 'NONE', *, *, #18251, .T. ) ;
#7680 = CARTESIAN_POINT ( 'NONE',  ( 12.46874999795161543, 3.632567103900569361, -3.270778111535288080 ) ) ;
#7681 = VECTOR ( 'NONE', #12209, 999.9999999999998863 ) ;
#7682 = CARTESIAN_POINT ( 'NONE',  ( 14.34374999795161365, 1.280903732194486722, -4.780397808154247308 ) ) ;
#7683 = EDGE_CURVE ( 'NONE', #12225, #8623, #19548, .T. ) ;
#7684 = CARTESIAN_POINT ( 'NONE',  ( 1.749999999999998002, -27.76164181293054511, 4.147968289691195132 ) ) ;
#7685 = DIRECTION ( 'NONE',  ( 0.000000000000000000, 0.000000000000000000, 1.000000000000000000 ) ) ;
#7686 = VERTEX_POINT ( 'NONE', #15192 ) ;
#7687 = CARTESIAN_POINT ( 'NONE',  ( 8.000000000000005329, 3.350375938067097437, -4.611396867937201272 ) ) ;
#7688 =( NAMED_UNIT ( * ) SI_UNIT ( $, .STERADIAN. ) SOLID_ANGLE_UNIT ( ) );
#7689 = CARTESIAN_POINT ( 'NONE',  ( 1.394999999999999574, -24.89775460606841406, 12.96210679857778025 ) ) ;
#7690 = DIRECTION ( 'NONE',  ( 0.000000000000000000, 0.000000000000000000, -1.000000000000000000 ) ) ;
#7691 = VERTEX_POINT ( 'NONE', #15886 ) ;
#7692 = CARTESIAN_POINT ( 'NONE',  ( 2.789999999999999147, -24.04302995059964587, -1.991882183130548878 ) ) ;
#7693 = AXIS2_PLACEMENT_3D ( 'NONE', #15152, #10554, #10751 ) ;
#7694 = CARTESIAN_POINT ( 'NONE',  ( -16.11901729331276911, 5.562305898749051458, -35.00000000000000000 ) ) ;
#7695 = CARTESIAN_POINT ( 'NONE',  ( 4.936344801571289409, -2.850000000000023626, -11.00000000000000711 ) ) ;
#7696 = CARTESIAN_POINT ( 'NONE',  ( -13.32184790671639618, 13.12143529358541549, -35.00000000000000000 ) ) ;
#7697 = ORIENTED_EDGE ( 'NONE', *, *, #9263, .T. ) ;
#7698 = DIRECTION ( 'NONE',  ( -0.000000000000000000, -0.000000000000000000, 1.000000000000000000 ) ) ;
#7699 = CARTESIAN_POINT ( 'NONE',  ( 0.02436607992776238310, -12.59161484032927092, 21.30679549418627161 ) ) ;
#7700 = EDGE_LOOP ( 'NONE', ( #12235, #15731 ) ) ;
#7701 = CARTESIAN_POINT ( 'NONE',  ( 11.96874999795161365, -4.888101187499994893, -0.7741991708319226895 ) ) ;
#7702 = EDGE_CURVE ( 'NONE', #10842, #10348, #2304, .T. ) ;
#7703 = FACE_OUTER_BOUND ( 'NONE', #8586, .T. ) ;
#7704 = ORIENTED_EDGE ( 'NONE', *, *, #1342, .F. ) ;
#7705 = EDGE_CURVE ( 'NONE', #9739, #12760, #7742, .T. ) ;
#7706 = AXIS2_PLACEMENT_3D ( 'NONE', #9829, #5101, #11215 ) ;
#7707 = AXIS2_PLACEMENT_3D ( 'NONE', #2607, #18035, #18228 ) ;
#7708 = VECTOR ( 'NONE', #2628, 1000.000000000000000 ) ;
#7709 = CARTESIAN_POINT ( 'NONE',  ( -4.888101187500000222, 0.7741991708318887166, -7.343749997951615427 ) ) ;
#7710 = CARTESIAN_POINT ( 'NONE',  ( 2.500000000000002220, 0.000000000000000000, 0.000000000000000000 ) ) ;
#7711 = EDGE_CURVE ( 'NONE', #126, #3453, #6440, .T. ) ;
#7712 = ORIENTED_EDGE ( 'NONE', *, *, #7953, .T. ) ;
#7713 = DIRECTION ( 'NONE',  ( 1.000000000000000000, -0.000000000000000000, 0.000000000000000000 ) ) ;
#7714 = CARTESIAN_POINT ( 'NONE',  ( 10.46874999795161720, 4.648860486681953397, -1.510506337161861667 ) ) ;
#7715 = EDGE_LOOP ( 'NONE', ( #8147, #15727 ) ) ;
#7716 = FACE_OUTER_BOUND ( 'NONE', #8750, .T. ) ;
#7717 = VERTEX_POINT ( 'NONE', #9693 ) ;
#7718 = FACE_OUTER_BOUND ( 'NONE', #11351, .T. ) ;
#7719 = ORIENTED_EDGE ( 'NONE', *, *, #5781, .T. ) ;
#7720 = FACE_OUTER_BOUND ( 'NONE', #4817, .T. ) ;
#7721 = CARTESIAN_POINT ( 'NONE',  ( -36.00000000000000000, 4.999999999999999112, -2.000000000000000000 ) ) ;
#7722 = EDGE_CURVE ( 'NONE', #4586, #3618, #10314, .T. ) ;
#7723 = VECTOR ( 'NONE', #19277, 1000.000000000000000 ) ;
#7724 = CIRCLE ( 'NONE', #389, 1.000000000000003553 ) ;
#7725 = DIRECTION ( 'NONE',  ( -1.000000000000000000, -0.000000000000000000, 0.000000000000000000 ) ) ;
#7726 = VERTEX_POINT ( 'NONE', #11081 ) ;
#7727 = AXIS2_PLACEMENT_3D ( 'NONE', #2507, #4313, #1310 ) ;
#7728 = DIRECTION ( 'NONE',  ( -1.000000000000000000, 0.000000000000000000, 0.000000000000000000 ) ) ;
#7729 = EDGE_CURVE ( 'NONE', #16827, #15303, #481, .T. ) ;
#7730 = DIRECTION ( 'NONE',  ( 0.000000000000000000, 0.000000000000000000, -1.000000000000000000 ) ) ;
#7731 = EDGE_CURVE ( 'NONE', #9581, #9713, #18599, .T. ) ;
#7732 = AXIS2_PLACEMENT_3D ( 'NONE', #6548, #18574, #8167 ) ;
#7733 = ORIENTED_EDGE ( 'NONE', *, *, #16716, .F. ) ;
#7734 = CARTESIAN_POINT ( 'NONE',  ( -41.99999999999999289, 4.999999999999998224, -2.000000000000000000 ) ) ;
#7735 = DIRECTION ( 'NONE',  ( 0.000000000000000000, 0.000000000000000000, 1.000000000000000000 ) ) ;
#7736 = ORIENTED_EDGE ( 'NONE', *, *, #7227, .T. ) ;
#7737 = VECTOR ( 'NONE', #10214, 1000.000000000000000 ) ;
#7738 = CARTESIAN_POINT ( 'NONE',  ( 2.601776091974071115, 25.40949241676360515, -5.251266773802107934 ) ) ;
#7739 = EDGE_CURVE ( 'NONE', #8597, #9421, #17652, .T. ) ;
#7740 = PRESENTATION_LAYER_ASSIGNMENT (  '', '', ( #2320 ) ) ;
#7741 = CARTESIAN_POINT ( 'NONE',  ( 7.937500000000000000, 4.582717761692648217, -6.527800000000000047 ) ) ;
#7742 = CIRCLE ( 'NONE', #7078, 1.000000000000000888 ) ;
#7743 =( NAMED_UNIT ( * ) PLANE_ANGLE_UNIT ( ) SI_UNIT ( $, .RADIAN. ) );
#7744 = VERTEX_POINT ( 'NONE', #8274 ) ;
#7745 = DIRECTION ( 'NONE',  ( -0.000000000000000000, -0.000000000000000000, 1.000000000000000000 ) ) ;
#7746 = ORIENTED_EDGE ( 'NONE', *, *, #16534, .T. ) ;
#7747 = APPLICATION_PROTOCOL_DEFINITION ( 'draft international standard', 'automotive_design', 1998, #13155 ) ;
#7748 = CARTESIAN_POINT ( 'NONE',  ( 1.749999999999998002, 12.96210679857822257, -24.89775460606818669 ) ) ;
#7749 = CARTESIAN_POINT ( 'NONE',  ( -2.318398865532109721, -5.207209108562803834, -10.31249999590322552 ) ) ;
#7750 = EDGE_CURVE ( 'NONE', #18923, #18527, #14834, .T. ) ;
#7751 = AXIS2_PLACEMENT_3D ( 'NONE', #11376, #14376, #14766 ) ;
#7752 = ORIENTED_EDGE ( 'NONE', *, *, #14032, .F. ) ;
#7753 = ORIENTED_EDGE ( 'NONE', *, *, #18156, .T. ) ;
#7754 = CARTESIAN_POINT ( 'NONE',  ( 2.849999999999954348, -4.936344801571327601, -6.656249997951614539 ) ) ;
#7755 = CARTESIAN_POINT ( 'NONE',  ( 6.468749997951615427, 4.233219804643871598, 2.444050593750020095 ) ) ;
#7756 = ORIENTED_EDGE ( 'NONE', *, *, #13377, .F. ) ;
#7757 = EDGE_CURVE ( 'NONE', #14026, #10153, #19253, .T. ) ;
#7758 = AXIS2_PLACEMENT_3D ( 'NONE', #11470, #2259, #14575 ) ;
#7759 = DIRECTION ( 'NONE',  ( -1.000000000000000000, 0.000000000000000000, 0.000000000000000000 ) ) ;
#7760 = ORIENTED_EDGE ( 'NONE', *, *, #19713, .F. ) ;
#7761 = VECTOR ( 'NONE', #10849, 1000.000000000000000 ) ;
#7762 = CIRCLE ( 'NONE', #19371, 24.12539914357697768 ) ;
#7763 = DIRECTION ( 'NONE',  ( 0.000000000000000000, 0.000000000000000000, 1.000000000000000000 ) ) ;
#7764 = CARTESIAN_POINT ( 'NONE',  ( 6.843749997951615427, 4.233219804643871598, 2.444050593750020095 ) ) ;
#7765 = DIRECTION ( 'NONE',  ( 0.000000000000000000, 0.000000000000000000, 1.000000000000000000 ) ) ;
#7766 = ORIENTED_EDGE ( 'NONE', *, *, #9565, .T. ) ;
#7767 = APPLICATION_CONTEXT ( 'automotive_design' ) ;
#7768 = EDGE_LOOP ( 'NONE', ( #14109, #2656, #69 ) ) ;
#7769 = CARTESIAN_POINT ( 'NONE',  ( 0.5279272933715191130, -18.56460150496952366, 19.66369668717026897 ) ) ;
#7770 = DIRECTION ( 'NONE',  ( 0.000000000000000000, 0.000000000000000000, 1.000000000000000000 ) ) ;
#7771 = ORIENTED_EDGE ( 'NONE', *, *, #17613, .F. ) ;
#7772 = VERTEX_POINT ( 'NONE', #12587 ) ;
#7773 = DIRECTION ( 'NONE',  ( -1.000000000000000000, 0.000000000000000000, 0.000000000000000000 ) ) ;
#7774 = CARTESIAN_POINT ( 'NONE',  ( 2.849999999999954348, -4.936344801571327601, -7.312499995903225525 ) ) ;
#7775 = DIRECTION ( 'NONE',  ( 1.000000000000000000, 0.000000000000000000, 0.000000000000000000 ) ) ;
#7776 = CIRCLE ( 'NONE', #18964, 1.000000000000003553 ) ;
#7777 = CARTESIAN_POINT ( 'NONE',  ( -2.255998204157477538, -17.85806462366060288, 32.00000000000000000 ) ) ;
#7778 = CARTESIAN_POINT ( 'NONE',  ( 1.761396867937200073, 5.421022142882376826, -12.00000000000000533 ) ) ;
#7779 = EDGE_CURVE ( 'NONE', #10940, #6746, #6854, .T. ) ;
#7780 = ORIENTED_EDGE ( 'NONE', *, *, #2356, .T. ) ;
#7781 = DIRECTION ( 'NONE',  ( -1.000000000000000000, 0.000000000000000000, 0.000000000000000000 ) ) ;
#7782 = CARTESIAN_POINT ( 'NONE',  ( 13.00000000000000000, -4.333424887442987483, -2.261628166637620119 ) ) ;
#7783 = EDGE_LOOP ( 'NONE', ( #13202, #5324 ) ) ;
#7784 = CARTESIAN_POINT ( 'NONE',  ( -11.00000000000000355, -3.278623949159158446, -2.625000000000002220 ) ) ;
#7785 = CARTESIAN_POINT ( 'NONE',  ( 8.343749997951611874, -4.942249507334558700, 0.2590123213420631454 ) ) ;
#7786 = EDGE_CURVE ( 'NONE', #3138, #17485, #13151, .T. ) ;
#7787 = AXIS2_PLACEMENT_3D ( 'NONE', #8342, #9274, #6722 ) ;
#7788 = CARTESIAN_POINT ( 'NONE',  ( -5.207209108562852684, -2.318398865532001363, -9.312499995903225525 ) ) ;
#7789 = FACE_OUTER_BOUND ( 'NONE', #12328, .T. ) ;
#7790 = ORIENTED_EDGE ( 'NONE', *, *, #6750, .T. ) ;
#7791 = CARTESIAN_POINT ( 'NONE',  ( 12.46874999795161543, 4.648860486681953397, 1.510506337161861223 ) ) ;
#7792 = CARTESIAN_POINT ( 'NONE',  ( 7.937499999999996447, -4.582717761692668645, -0.7089489049740167470 ) ) ;
#7793 = CYLINDRICAL_SURFACE ( 'NONE', #10573, 9.000000000000000000 ) ;
#7794 = ORIENTED_EDGE ( 'NONE', *, *, #12939, .F. ) ;
#7795 = CARTESIAN_POINT ( 'NONE',  ( 5.700000000000001066, -0.2987243419133416289, -12.83455515208547304 ) ) ;
#7796 = TOROIDAL_SURFACE ( 'NONE', #4289, 7.800000000000000711, 0.1999999999999998723 ) ;
#7797 = CARTESIAN_POINT ( 'NONE',  ( 0.000000000000000000, 0.000000000000000000, 7.500000000000000000 ) ) ;
#7798 = CARTESIAN_POINT ( 'NONE',  ( 13.50000000000000533, -1.493657965219523209, 5.574407415329156734 ) ) ;
#7799 = DIRECTION ( 'NONE',  ( 0.000000000000000000, 0.000000000000000000, -1.000000000000000000 ) ) ;
#7800 = EDGE_LOOP ( 'NONE', ( #18272, #7636 ) ) ;
#7801 = CARTESIAN_POINT ( 'NONE',  ( 0.02436607992775674525, 9.836394144776026138, -22.71065055754441531 ) ) ;
#7802 = CARTESIAN_POINT ( 'NONE',  ( -3.499494075959816541, 3.499494075959816541, -9.343749997951615427 ) ) ;
#7803 = EDGE_CURVE ( 'NONE', #16718, #11385, #4509, .T. ) ;
#7804 = ORIENTED_EDGE ( 'NONE', *, *, #5407, .F. ) ;
#7805 = AXIS2_PLACEMENT_3D ( 'NONE', #6185, #16820, #12311 ) ;
#7806 = CARTESIAN_POINT ( 'NONE',  ( -1.869200000000000195, 0.000000000000000000, 0.000000000000000000 ) ) ;
#7807 = FACE_OUTER_BOUND ( 'NONE', #395, .T. ) ;
#7808 = ADVANCED_BREP_SHAPE_REPRESENTATION ( '', ( #2634, #16724 ), #12592 ) ;
#7809 = ORIENTED_EDGE ( 'NONE', *, *, #16674, .F. ) ;
#7810 = COLOUR_RGB ( '', 0.66274510, 0.83137255, 0.94901961) ;
#7811 = LINE ( 'NONE', #18815, #3242 ) ;
#7812 = LINE ( 'NONE', #15822, #8196 ) ;
#7813 = ORIENTED_EDGE ( 'NONE', *, *, #11844, .F. ) ;
#7814 = DIRECTION ( 'NONE',  ( 1.000000000000000000, 0.000000000000000000, 0.000000000000000000 ) ) ;
#7815 = DIRECTION ( 'NONE',  ( 0.000000000000000000, 0.000000000000000000, -1.000000000000000000 ) ) ;
#7816 = CIRCLE ( 'NONE', #5265, 4.200000000000000178 ) ;
#7817 = EDGE_LOOP ( 'NONE', ( #16531, #11155 ) ) ;
#7818 = EDGE_CURVE ( 'NONE', #5672, #17130, #2915, .T. ) ;
#7819 = DIRECTION ( 'NONE',  ( -1.000000000000000000, 0.000000000000000000, 0.000000000000000000 ) ) ;
#7820 = ORIENTED_EDGE ( 'NONE', *, *, #4736, .T. ) ;
#7821 = EDGE_CURVE ( 'NONE', #4759, #7944, #3670, .T. ) ;
#7822 = CARTESIAN_POINT ( 'NONE',  ( -4.476417968967385974, 17.43449690031536292, -35.00000000000000000 ) ) ;
#7823 = ORIENTED_EDGE ( 'NONE', *, *, #8558, .F. ) ;
#7824 = CARTESIAN_POINT ( 'NONE',  ( -5.000000000000000000, 1.999999999999998668, 37.99999999999999289 ) ) ;
#7825 = CYLINDRICAL_SURFACE ( 'NONE', #16856, 1.000000000000003553 ) ;
#7826 = AXIS2_PLACEMENT_3D ( 'NONE', #10287, #2760, #8577 ) ;
#7827 = LINE ( 'NONE', #29, #4093 ) ;
#7828 = ORIENTED_EDGE ( 'NONE', *, *, #17501, .F. ) ;
#7829 = CARTESIAN_POINT ( 'NONE',  ( -36.00000000000000000, -2.311115933264683024E-31, 0.000000000000000000 ) ) ;
#7830 = DIRECTION ( 'NONE',  ( 0.5877852522924679191, -0.8090169943749512260, 0.000000000000000000 ) ) ;
#7831 = ORIENTED_EDGE ( 'NONE', *, *, #11409, .F. ) ;
#7832 = DIRECTION ( 'NONE',  ( 0.000000000000000000, 0.000000000000000000, 1.000000000000000000 ) ) ;
#7833 = DIRECTION ( 'NONE',  ( -1.000000000000000000, -0.000000000000000000, -0.000000000000000000 ) ) ;
#7834 = VERTEX_POINT ( 'NONE', #582 ) ;
#7835 = TOROIDAL_SURFACE ( 'NONE', #519, 24.12539914357697413, 8.000000000000000000 ) ;
#7836 = CARTESIAN_POINT ( 'NONE',  ( 2.999999999999998224, 3.950217066951266176, 3.681818181818181213 ) ) ;
#7837 = DIRECTION ( 'NONE',  ( -1.000000000000000000, -1.224646799147353207E-16, 0.000000000000000000 ) ) ;
#7838 = AXIS2_PLACEMENT_3D ( 'NONE', #13670, #16781, #8872 ) ;
#7839 = VERTEX_POINT ( 'NONE', #5163 ) ;
#7840 = CARTESIAN_POINT ( 'NONE',  ( 13.00000000000000000, -0.2080849974988778772, -4.883670121236158401 ) ) ;
#7841 = EDGE_LOOP ( 'NONE', ( #13790, #9790, #2797, #15626 ) ) ;
#7842 = PRODUCT_CONTEXT ( 'NONE', #8430, 'mechanical' ) ;
#7843 = DIRECTION ( 'NONE',  ( 0.9238795325112865164, -0.3826834323650905034, 0.000000000000000000 ) ) ;
#7844 = FACE_OUTER_BOUND ( 'NONE', #8339, .T. ) ;
#7845 = ORIENTED_EDGE ( 'NONE', *, *, #15670, .T. ) ;
#7846 = ORIENTED_EDGE ( 'NONE', *, *, #13962, .F. ) ;
#7847 = CARTESIAN_POINT ( 'NONE',  ( 0.7589665349472715095, 27.14933624560914893, -4.828387785247743480 ) ) ;
#7848 = CARTESIAN_POINT ( 'NONE',  ( 5.575441324182695446, 1.185096637661216201, -13.31249999590322730 ) ) ;
#7849 = ORIENTED_EDGE ( 'NONE', *, *, #17638, .T. ) ;
#7850 = ADVANCED_FACE ( 'NONE', ( #14384 ), #680, .F. ) ;
#7851 = EDGE_CURVE ( 'NONE', #17509, #7960, #6489, .T. ) ;
#7852 = AXIS2_PLACEMENT_3D ( 'NONE', #2815, #15033, #12034 ) ;
#7853 = CARTESIAN_POINT ( 'NONE',  ( 1.039999999999997593, 0.000000000000000000, 0.000000000000000000 ) ) ;
#7854 = ORIENTED_EDGE ( 'NONE', *, *, #4814, .T. ) ;
#7855 = EDGE_CURVE ( 'NONE', #5327, #18865, #18206, .T. ) ;
#7856 = CARTESIAN_POINT ( 'NONE',  ( -3.814044456245531567, -4.235925505221111997, -10.00000000000000533 ) ) ;
#7857 = CARTESIAN_POINT ( 'NONE',  ( -11.00000000000000355, 3.278623949159158446, -2.625000000000002220 ) ) ;
#7858 = CARTESIAN_POINT ( 'NONE',  ( 1.039999999999996039, 27.68468304288258963, 4.633866840649018215 ) ) ;
#7859 = AXIS2_PLACEMENT_3D ( 'NONE', #3295, #1793, #7885 ) ;
#7860 = EDGE_LOOP ( 'NONE', ( #3895, #1558, #24, #8566 ) ) ;
#7861 = CARTESIAN_POINT ( 'NONE',  ( 3.255998204157476206, -17.85806462366060288, -32.00000000000000000 ) ) ;
#7862 = EDGE_CURVE ( 'NONE', #1573, #9163, #7052, .T. ) ;
#7863 = FACE_OUTER_BOUND ( 'NONE', #12012, .T. ) ;
#7864 = EDGE_LOOP ( 'NONE', ( #2649, #16659, #3516, #13525 ) ) ;
#7865 = EDGE_LOOP ( 'NONE', ( #4861, #12948, #19515, #18277 ) ) ;
#7866 = DIRECTION ( 'NONE',  ( -0.000000000000000000, 0.000000000000000000, 1.000000000000000000 ) ) ;
#7867 = DIRECTION ( 'NONE',  ( 1.000000000000000000, 6.419766481290786633E-33, -0.000000000000000000 ) ) ;
#7868 = CARTESIAN_POINT ( 'NONE',  ( -34.92499999999994742, 0.000000000000000000, 0.000000000000000000 ) ) ;
#7869 = DIRECTION ( 'NONE',  ( 0.000000000000000000, 1.000000000000000000, 0.000000000000000000 ) ) ;
#7870 = CARTESIAN_POINT ( 'NONE',  ( -3.490243377569957047E-16, 5.700000000000001066, -11.00000000000000711 ) ) ;
#7871 = EDGE_LOOP ( 'NONE', ( #19739, #8895, #1836, #17867 ) ) ;
#7872 = DIRECTION ( 'NONE',  ( -0.000000000000000000, -0.000000000000000000, 1.000000000000000000 ) ) ;
#7873 = CYLINDRICAL_SURFACE ( 'NONE', #16841, 1.000000000000000888 ) ;
#7874 = CIRCLE ( 'NONE', #19066, 3.000000000000000000 ) ;
#7875 = ORIENTED_EDGE ( 'NONE', *, *, #17394, .F. ) ;
#7876 = CARTESIAN_POINT ( 'NONE',  ( -17.68117051311639898, -3.372863662543042818, 32.00000000000000000 ) ) ;
#7877 = AXIS2_PLACEMENT_3D ( 'NONE', #7710, #4619, #1525 ) ;
#7878 = EDGE_CURVE ( 'NONE', #8143, #12225, #1541, .T. ) ;
#7879 = CARTESIAN_POINT ( 'NONE',  ( 0.02436607992776325046, -18.55949924794904504, 16.37294372382852004 ) ) ;
#7880 = CARTESIAN_POINT ( 'NONE',  ( -5.700000000000001066, 1.090170143537592985E-15, -10.64522241986045259 ) ) ;
#7881 = DIRECTION ( 'NONE',  ( -1.000000000000000000, -0.000000000000000000, -0.000000000000000000 ) ) ;
#7882 = FACE_OUTER_BOUND ( 'NONE', #10257, .T. ) ;
#7883 = ORIENTED_EDGE ( 'NONE', *, *, #16920, .T. ) ;
#7884 = EDGE_CURVE ( 'NONE', #18970, #9059, #9692, .T. ) ;
#7885 = DIRECTION ( 'NONE',  ( 0.000000000000000000, 0.000000000000000000, 1.000000000000000000 ) ) ;
#7886 = SURFACE_STYLE_USAGE ( .BOTH. , #199 ) ;
#7887 = CARTESIAN_POINT ( 'NONE',  ( -10.99900000000000233, -7.061101152771736665E-32, 0.000000000000000000 ) ) ;
#7888 = DIRECTION ( 'NONE',  ( 0.000000000000000000, 0.000000000000000000, 1.000000000000000000 ) ) ;
#7889 = ORIENTED_EDGE ( 'NONE', *, *, #16802, .T. ) ;
#7890 = FACE_OUTER_BOUND ( 'NONE', #13575, .T. ) ;
#7891 = VECTOR ( 'NONE', #6748, 1000.000000000000000 ) ;
#7892 = FACE_OUTER_BOUND ( 'NONE', #12635, .T. ) ;
#7893 = CARTESIAN_POINT ( 'NONE',  ( 10.00000000000000533, 4.235925505221138643, 3.814044456245502701 ) ) ;
#7894 = AXIS2_PLACEMENT_3D ( 'NONE', #6480, #510, #6194 ) ;
#7895 = DIRECTION ( 'NONE',  ( 1.000000000000000000, 0.000000000000000000, 0.000000000000000000 ) ) ;
#7896 = ORIENTED_EDGE ( 'NONE', *, *, #9623, .T. ) ;
#7897 = DIRECTION ( 'NONE',  ( 0.000000000000000000, 0.000000000000000000, 1.000000000000000000 ) ) ;
#7898 = DIRECTION ( 'NONE',  ( 0.000000000000000000, 0.000000000000000000, -1.000000000000000000 ) ) ;
#7899 = ORIENTED_EDGE ( 'NONE', *, *, #3515, .T. ) ;
#7900 = CARTESIAN_POINT ( 'NONE',  ( 12.34374999795161543, -4.888101187499994893, -0.7741991708319226895 ) ) ;
#7901 = DIRECTION ( 'NONE',  ( 0.000000000000000000, 0.000000000000000000, -1.000000000000000000 ) ) ;
#7902 = ORIENTED_EDGE ( 'NONE', *, *, #783, .T. ) ;
#7903 = EDGE_CURVE ( 'NONE', #17130, #9276, #12218, .T. ) ;
#7904 = CIRCLE ( 'NONE', #18763, 4.400000000000000355 ) ;
#7905 = AXIS2_PLACEMENT_3D ( 'NONE', #10522, #16618, #2900 ) ;
#7906 = FACE_OUTER_BOUND ( 'NONE', #11724, .T. ) ;
#7907 = DIRECTION ( 'NONE',  ( 0.000000000000000000, 0.000000000000000000, 1.000000000000000000 ) ) ;
#7908 = VERTEX_POINT ( 'NONE', #4534 ) ;
#7909 = CARTESIAN_POINT ( 'NONE',  ( 0.000000000000000000, 18.28042085475278000, 15.74360496233386719 ) ) ;
#7910 = CARTESIAN_POINT ( 'NONE',  ( -0.7741991708318890497, 4.888101187500000222, -10.96874999795161720 ) ) ;
#7911 = EDGE_CURVE ( 'NONE', #5740, #13049, #6127, .T. ) ;
#7912 = EDGE_LOOP ( 'NONE', ( #15261, #17283, #4714, #18710 ) ) ;
#7913 = CARTESIAN_POINT ( 'NONE',  ( 2.789999999999999147, 7.909232158574813099, 24.34211360614303388 ) ) ;
#7914 = ORIENTED_EDGE ( 'NONE', *, *, #15222, .F. ) ;
#7915 =( BOUNDED_SURFACE ( )  B_SPLINE_SURFACE ( 1, 2, ( 
 ( #13472, #19475, #13577, #4376, #19675, #1473, #4571, #19575, #1177, #12177, #16585, #14885, #11979, #9082, #15180, #17883, #8782 ),
 ( #7252, #17989, #7559, #16384, #10390, #2865, #13678, #16489, #18283, #5668, #10681, #16788, #1080, #15083, #2764, #7155, #19378 ) ),
 .UNSPECIFIED., .F., .F., .F. ) 
 B_SPLINE_SURFACE_WITH_KNOTS ( ( 2, 2 ),
 ( 3, 2, 2, 2, 2, 2, 2, 2, 3 ),
 ( 0.000000000000000000, 1.000000000000000000 ),
 ( 0.000000000000000000, 0.05000000000000000278, 0.1000000000000000056, 0.1499999999999999944, 0.2000000000000000111, 0.2500000000000000000, 0.2999999999999999889, 0.3499999999999999778, 0.4000000000000000222 ),
 .UNSPECIFIED. ) 
 GEOMETRIC_REPRESENTATION_ITEM ( )  RATIONAL_B_SPLINE_SURFACE ( (
 ( 1.000000000000000000, 0.9876883405951377704, 1.000000000000000000, 0.9876883405951377704, 1.000000000000000000, 0.9876883405951377704, 1.000000000000000000, 0.9876883405951377704, 1.000000000000000000, 0.9876883405951377704, 1.000000000000000000, 0.9876883405951377704, 1.000000000000000000, 0.9876883405951377704, 1.000000000000000000, 0.9876883405951377704, 1.000000000000000000),
 ( 1.000000000000000000, 0.9876883405951377704, 1.000000000000000000, 0.9876883405951377704, 1.000000000000000000, 0.9876883405951377704, 1.000000000000000000, 0.9876883405951377704, 1.000000000000000000, 0.9876883405951377704, 1.000000000000000000, 0.9876883405951377704, 1.000000000000000000, 0.9876883405951377704, 1.000000000000000000, 0.9876883405951377704, 1.000000000000000000) ) ) 
 REPRESENTATION_ITEM ( '' )  SURFACE ( )  );
#7916 = CARTESIAN_POINT ( 'NONE',  ( 2.718131914667132776, -23.19485392143220182, 10.24630254990507083 ) ) ;
#7917 = ORIENTED_EDGE ( 'NONE', *, *, #5218, .F. ) ;
#7918 = CARTESIAN_POINT ( 'NONE',  ( 0.000000000000000000, 0.000000000000000000, -33.00000000000000000 ) ) ;
#7919 = CARTESIAN_POINT ( 'NONE',  ( 0.000000000000000000, 0.000000000000000000, 32.00000000000000000 ) ) ;
#7920 = DIRECTION ( 'NONE',  ( 0.000000000000000000, 0.000000000000000000, -1.000000000000000000 ) ) ;
#7921 = AXIS2_PLACEMENT_3D ( 'NONE', #3400, #9511, #12703 ) ;
#7922 = CARTESIAN_POINT ( 'NONE',  ( -5.700000000000001066, 0.000000000000000000, -6.000000000000005329 ) ) ;
#7923 = CIRCLE ( 'NONE', #15605, 22.00000000000000355 ) ;
#7924 = ORIENTED_EDGE ( 'NONE', *, *, #15785, .F. ) ;
#7925 = LINE ( 'NONE', #14136, #19567 ) ;
#7926 = DIRECTION ( 'NONE',  ( 1.000000000000000000, 0.000000000000000000, 0.000000000000000000 ) ) ;
#7927 = EDGE_CURVE ( 'NONE', #13729, #8384, #10641, .T. ) ;
#7928 = ORIENTED_EDGE ( 'NONE', *, *, #6998, .T. ) ;
#7929 = B_SPLINE_CURVE_WITH_KNOTS ( 'NONE', 3,
 ( #6647, #17377, #3662, #9787, #15879, #16743 ),
 .UNSPECIFIED., .F., .F.,
 ( 4, 2, 4 ),
 ( 4.462636695690012598E-07, 0.001879885036799766119, 0.003759323809929963553 ),
 .UNSPECIFIED. ) ;
#7930 = FACE_OUTER_BOUND ( 'NONE', #4361, .T. ) ;
#7931 = FACE_OUTER_BOUND ( 'NONE', #1907, .T. ) ;
#7932 = VECTOR ( 'NONE', #16874, 1000.000000000000000 ) ;
#7933 = ORIENTED_EDGE ( 'NONE', *, *, #18788, .T. ) ;
#7934 = DIRECTION ( 'NONE',  ( 0.000000000000000000, 0.000000000000000000, -1.000000000000000000 ) ) ;
#7935 = CARTESIAN_POINT ( 'NONE',  ( 13.84374999795161543, 4.465502636338051445, -1.988169868018530906 ) ) ;
#7936 = EDGE_CURVE ( 'NONE', #7585, #9689, #8992, .T. ) ;
#7937 = EDGE_LOOP ( 'NONE', ( #12356, #6834, #5145, #5339, #12057 ) ) ;
#7938 = DIRECTION ( 'NONE',  ( -1.000000000000000000, 0.000000000000000000, 0.000000000000000000 ) ) ;
#7939 = ORIENTED_EDGE ( 'NONE', *, *, #9972, .T. ) ;
#7940 = SHAPE_DEFINITION_REPRESENTATION ( #14506, #2475 ) ;
#7941 = CARTESIAN_POINT ( 'NONE',  ( 2.718131853594927261, 12.74240566899015903, -21.92302674874949986 ) ) ;
#7942 = AXIS2_PLACEMENT_3D ( 'NONE', #15267, #12162, #13451 ) ;
#7943 = CARTESIAN_POINT ( 'NONE',  ( 12.46874999795161543, 1.016293382781411792, 4.781284448697194378 ) ) ;
#7944 = VERTEX_POINT ( 'NONE', #1240 ) ;
#7945 = ORIENTED_EDGE ( 'NONE', *, *, #127, .T. ) ;
#7946 = CARTESIAN_POINT ( 'NONE',  ( 0.7592463896980118365, -19.12676442129330212, -19.86438386685682644 ) ) ;
#7947 = CARTESIAN_POINT ( 'NONE',  ( -9.000000000000000000, 0.000000000000000000, -29.00000000000000000 ) ) ;
#7948 = EDGE_LOOP ( 'NONE', ( #4368, #8565, #12594, #6482 ) ) ;
#7949 = CIRCLE ( 'NONE', #9569, 6.000000000000000888 ) ;
#7950 = CARTESIAN_POINT ( 'NONE',  ( 7.937500000000000000, -4.582717761692665981, -6.527800000000000047 ) ) ;
#7951 = ADVANCED_FACE ( 'NONE', ( #16088 ), #10546, .F. ) ;
#7952 = VERTEX_POINT ( 'NONE', #4440 ) ;
#7953 = EDGE_CURVE ( 'NONE', #19421, #19054, #13644, .T. ) ;
#7954 = CARTESIAN_POINT ( 'NONE',  ( 15.19790265903627358, 9.644882309621939598, -32.00000000000000000 ) ) ;
#7955 = FACE_BOUND ( 'NONE', #12888, .T. ) ;
#7956 = EDGE_CURVE ( 'NONE', #2077, #3033, #14148, .T. ) ;
#7957 = ORIENTED_EDGE ( 'NONE', *, *, #429, .F. ) ;
#7958 = DIRECTION ( 'NONE',  ( 1.000000000000000000, 1.224646799147353207E-16, -0.000000000000000000 ) ) ;
#7959 = CARTESIAN_POINT ( 'NONE',  ( 8.000000000000000000, 0.000000000000000000, 0.000000000000000000 ) ) ;
#7960 = VERTEX_POINT ( 'NONE', #19647 ) ;
#7961 = ORIENTED_EDGE ( 'NONE', *, *, #4603, .T. ) ;
#7962 = CYLINDRICAL_SURFACE ( 'NONE', #12422, 4.200000000000000178 ) ;
#7963 = DIRECTION ( 'NONE',  ( 1.000000000000000000, 0.000000000000000000, 0.000000000000000000 ) ) ;
#7964 =( GEOMETRIC_REPRESENTATION_CONTEXT ( 3 ) GLOBAL_UNCERTAINTY_ASSIGNED_CONTEXT ( ( #6973 ) ) GLOBAL_UNIT_ASSIGNED_CONTEXT ( ( #15700, #10004, #16105 ) ) REPRESENTATION_CONTEXT ( 'NONE', 'WORKASPACE' ) );
#7965 = CARTESIAN_POINT ( 'NONE',  ( 2.647025296874957689, -4.584782303107616031, -6.234374998975811266 ) ) ;
#7966 = B_SPLINE_CURVE_WITH_KNOTS ( 'NONE', 3,
 ( #3491, #291, #12499, #6372 ),
 .UNSPECIFIED., .F., .F.,
 ( 4, 4 ),
 ( 0.005258214619651976202, 0.005948481662034167325 ),
 .UNSPECIFIED. ) ;
#7968 = EDGE_CURVE ( 'NONE', #8477, #16209, #15062, .T. ) ;
#7967 = SHAPE_REPRESENTATION ( 'Internal Brake Shoe', ( #16724 ), #6818 ) ;
#7969 = EDGE_CURVE ( 'NONE', #18235, #10647, #7412, .T. ) ;
#7970 = CARTESIAN_POINT ( 'NONE',  ( -90.00000000000000000, 1.012170579495290078E-15, 8.265000000000021885 ) ) ;
#7971 = CARTESIAN_POINT ( 'NONE',  ( -5.421022142882375938, 1.761396867937200517, -7.000000000000005329 ) ) ;
#7972 = ORIENTED_EDGE ( 'NONE', *, *, #615, .T. ) ;
#7973 = DIRECTION ( 'NONE',  ( 0.000000000000000000, 1.000000000000000000, 1.099230717450651647E-14 ) ) ;
#7974 = CARTESIAN_POINT ( 'NONE',  ( -1.001543065824775120E-15, -9.165435523385328409, -6.527800000000000047 ) ) ;
#7975 = EDGE_LOOP ( 'NONE', ( #14028, #18041 ) ) ;
#7976 = CARTESIAN_POINT ( 'NONE',  ( 4.465502636338025688, -1.988169868018592856, -14.46874999795161720 ) ) ;
#7977 = EDGE_CURVE ( 'NONE', #2077, #4951, #5833, .T. ) ;
#7978 = CARTESIAN_POINT ( 'NONE',  ( 11.84374999795161365, -2.444050593749961031, -4.233219804643904460 ) ) ;
#7979 = CIRCLE ( 'NONE', #15979, 4.000000000000000000 ) ;
#7980 = AXIS2_PLACEMENT_3D ( 'NONE', #10347, #4133, #2620 ) ;
#7981 = FACE_OUTER_BOUND ( 'NONE', #3484, .T. ) ;
#7982 = LINE ( 'NONE', #3583, #2658 ) ;
#7983 = CARTESIAN_POINT ( 'NONE',  ( 7.343749997951615427, 4.620319390059830056, -1.773574444220725521 ) ) ;
#7984 = ORIENTED_EDGE ( 'NONE', *, *, #13484, .T. ) ;
#7985 = CARTESIAN_POINT ( 'NONE',  ( 1.824075699840007170, -24.74770846292491910, 12.96726489871182153 ) ) ;
#7986 =( NAMED_UNIT ( * ) SI_UNIT ( $, .STERADIAN. ) SOLID_ANGLE_UNIT ( ) );
#7987 = CYLINDRICAL_SURFACE ( 'NONE', #12945, 13.19999999999999929 ) ;
#7988 = CARTESIAN_POINT ( 'NONE',  ( 91.50000000000000000, 0.000000000000000000, 0.000000000000000000 ) ) ;
#7989 = ORIENTED_EDGE ( 'NONE', *, *, #12130, .F. ) ;
#7990 = CARTESIAN_POINT ( 'NONE',  ( 8.000000000000000000, 0.000000000000000000, 0.000000000000000000 ) ) ;
#7991 = FACE_BOUND ( 'NONE', #10482, .T. ) ;
#7992 = LINE ( 'NONE', #12318, #663 ) ;
#7993 = CYLINDRICAL_SURFACE ( 'NONE', #1819, 8.073750000000021743 ) ;
#7994 = CARTESIAN_POINT ( 'NONE',  ( -2.850000000000058265, -4.936344801571268093, -6.000000000000005329 ) ) ;
#7995 = ORIENTED_EDGE ( 'NONE', *, *, #19101, .F. ) ;
#7996 = CARTESIAN_POINT ( 'NONE',  ( 2.789999999999999147, -23.48180575137734039, 5.535312321042630934 ) ) ;
#7997 = CIRCLE ( 'NONE', #9614, 4.200000000000000178 ) ;
#7998 = CARTESIAN_POINT ( 'NONE',  ( 2.788134175425139194, -20.90825775245756191, -12.51925356660783528 ) ) ;
#7999 = AXIS2_PLACEMENT_3D ( 'NONE', #18600, #18311, #1704 ) ;
#8000 = ORIENTED_EDGE ( 'NONE', *, *, #591, .T. ) ;
#8001 = CARTESIAN_POINT ( 'NONE',  ( 13.00000000000000000, 3.840809689103004576, -4.211671987713725862 ) ) ;
#8002 = CARTESIAN_POINT ( 'NONE',  ( -10.00000000000000000, 0.000000000000000000, 0.000000000000000000 ) ) ;
#8003 = ORIENTED_EDGE ( 'NONE', *, *, #3554, .T. ) ;
#8004 = FACE_BOUND ( 'NONE', #6260, .T. ) ;
#8005 = CARTESIAN_POINT ( 'NONE',  ( 5.510910596163084625E-16, 18.00000000000000355, -32.00000000000000000 ) ) ;
#8006 = VERTEX_POINT ( 'NONE', #10452 ) ;
#8007 = CIRCLE ( 'NONE', #5758, 9.000000000000000000 ) ;
#8008 = CARTESIAN_POINT ( 'NONE',  ( -16.11901729331276911, 5.562305898749051458, 32.00000000000000000 ) ) ;
#8009 = CARTESIAN_POINT ( 'NONE',  ( -2.993098736590125853E-16, 4.888101187500000222, -11.46874999795161543 ) ) ;
#8010 = ORIENTED_EDGE ( 'NONE', *, *, #1576, .F. ) ;
#8011 = DIRECTION ( 'NONE',  ( -0.000000000000000000, -0.000000000000000000, -1.000000000000000000 ) ) ;
#8012 = VERTEX_POINT ( 'NONE', #2830 ) ;
#8013 = DIRECTION ( 'NONE',  ( -7.654042494670960318E-17, 0.6250000000000002220, 0.7806247497997995666 ) ) ;
#8014 = VERTEX_POINT ( 'NONE', #8945 ) ;
#8015 = CARTESIAN_POINT ( 'NONE',  ( 0.02436607992776411782, 22.71065055754465689, -9.836394144775473691 ) ) ;
#8016 = CARTESIAN_POINT ( 'NONE',  ( 0.2590123213420631454, -4.942249507334558700, -8.343749997951611874 ) ) ;
#8017 = FACE_OUTER_BOUND ( 'NONE', #141, .T. ) ;
#8018 = CARTESIAN_POINT ( 'NONE',  ( 4.465502636338039011, 1.988169868018562436, -8.468749997951615427 ) ) ;
#8019 = ORIENTED_EDGE ( 'NONE', *, *, #6949, .T. ) ;
#8020 = DIRECTION ( 'NONE',  ( -1.000000000000000000, 0.000000000000000000, 0.000000000000000000 ) ) ;
#8021 = CARTESIAN_POINT ( 'NONE',  ( 0.8944271909999177428, 0.000000000000000000, 0.000000000000000000 ) ) ;
#8022 = ORIENTED_EDGE ( 'NONE', *, *, #5024, .T. ) ;
#8023 = ADVANCED_FACE ( 'NONE', ( #13543 ), #5929, .F. ) ;
#8024 = AXIS2_PLACEMENT_3D ( 'NONE', #11940, #7413, #6215 ) ;
#8025 = LINE ( 'NONE', #742, #9041 ) ;
#8026 = B_SPLINE_CURVE_WITH_KNOTS ( 'NONE', 3,
 ( #2058, #10974, #18471, #4966 ),
 .UNSPECIFIED., .F., .F.,
 ( 4, 4 ),
 ( 3.059063720746923042E-07, 0.0006888942284913959508 ),
 .UNSPECIFIED. ) ;
#8027 = CARTESIAN_POINT ( 'NONE',  ( -20.63749999999999929, 5.908920805885978590E-16, 4.824999999999999289 ) ) ;
#8028 = CARTESIAN_POINT ( 'NONE',  ( 1.394999999999998685, 24.89775460606832524, 12.96210679857795256 ) ) ;
#8029 = ORIENTED_EDGE ( 'NONE', *, *, #11239, .F. ) ;
#8030 = DIRECTION ( 'NONE',  ( 0.000000000000000000, 0.000000000000000000, -1.000000000000000000 ) ) ;
#8031 = ADVANCED_FACE ( 'NONE', ( #2929 ), #9045, .F. ) ;
#8032 = DIRECTION ( 'NONE',  ( -0.8660254037844380415, 0.5000000000000009992, 0.000000000000000000 ) ) ;
#8033 = ORIENTED_EDGE ( 'NONE', *, *, #4637, .T. ) ;
#8034 = DIRECTION ( 'NONE',  ( 1.000000000000000000, 1.224646799147353207E-16, -0.000000000000000000 ) ) ;
#8035 = CIRCLE ( 'NONE', #4529, 1.000000000000003109 ) ;
#8036 = ORIENTED_EDGE ( 'NONE', *, *, #790, .T. ) ;
#8037 = APPLICATION_PROTOCOL_DEFINITION ( 'draft international standard', 'automotive_design', 1998, #16226 ) ;
#8038 = CARTESIAN_POINT ( 'NONE',  ( -0.000000000000000000, 0.000000000000000000, 0.000000000000000000 ) ) ;
#8039 = PLANE ( 'NONE',  #19506 ) ;
#8040 = TOROIDAL_SURFACE ( 'NONE', #2928, 24.12539914357697768, 8.000000000000000000 ) ;
#8041 = ORIENTED_EDGE ( 'NONE', *, *, #13088, .F. ) ;
#8042 = VERTEX_POINT ( 'NONE', #234 ) ;
#8043 = DIRECTION ( 'NONE',  ( -0.000000000000000000, -0.000000000000000000, 1.000000000000000000 ) ) ;
#8044 = CARTESIAN_POINT ( 'NONE',  ( -12.86923836996420611, -11.47363181547641275, -32.00000000000000000 ) ) ;
#8045 = ORIENTED_EDGE ( 'NONE', *, *, #13728, .F. ) ;
#8046 = ADVANCED_FACE ( 'NONE', ( #13942 ), #17142, .T. ) ;
#8047 = CARTESIAN_POINT ( 'NONE',  ( -4.150607464521828938, -2.695436003842674122, -8.343749997951613651 ) ) ;
#8048 = ADVANCED_BREP_SHAPE_REPRESENTATION ( '', ( #2965, #16724 ), #16405 ) ;
#8049 = AXIS2_PLACEMENT_3D ( 'NONE', #8186, #5080, #11193 ) ;
#8050 = ORIENTED_EDGE ( 'NONE', *, *, #18223, .F. ) ;
#8051 = CIRCLE ( 'NONE', #5495, 1.000000000000002442 ) ;
#8052 = CIRCLE ( 'NONE', #9356, 1.000000000000002665 ) ;
#8053 = FACE_OUTER_BOUND ( 'NONE', #18288, .T. ) ;
#8054 = AXIS2_PLACEMENT_3D ( 'NONE', #1424, #7610, #19519 ) ;
#8055 = AXIS2_PLACEMENT_3D ( 'NONE', #9464, #18652, #15559 ) ;
#8056 = DIRECTION ( 'NONE',  ( -9.559896011775280412E-17, 0.7806247497997995666, -0.6250000000000002220 ) ) ;
#8057 = FACE_BOUND ( 'NONE', #18921, .T. ) ;
#8058 = EDGE_LOOP ( 'NONE', ( #7854, #4216, #5444, #16406 ) ) ;
#8059 = LINE ( 'NONE', #9578, #565 ) ;
#8060 = SURFACE_STYLE_FILL_AREA ( #15677 ) ;
#8061 = CARTESIAN_POINT ( 'NONE',  ( -3.000000000000002665, 0.000000000000000000, 6.000000000000000000 ) ) ;
#8062 = ORIENTED_EDGE ( 'NONE', *, *, #13748, .F. ) ;
#8063 = ADVANCED_FACE ( 'NONE', ( #15545 ), #3230, .T. ) ;
#8064 = ORIENTED_EDGE ( 'NONE', *, *, #10080, .T. ) ;
#8065 = FACE_OUTER_BOUND ( 'NONE', #13725, .T. ) ;
#8066 = ADVANCED_FACE ( 'NONE', ( #10942, #17048 ), #438, .T. ) ;
#8067 = AXIS2_PLACEMENT_3D ( 'NONE', #5864, #16383, #2663 ) ;
#8068 = VECTOR ( 'NONE', #6220, 1000.000000000000000 ) ;
#8069 = CARTESIAN_POINT ( 'NONE',  ( 2.765633920072239071, -16.37294372382844543, -18.55949924794910544 ) ) ;
#8070 = EDGE_CURVE ( 'NONE', #13082, #14863, #3923, .T. ) ;
#8071 = AXIS2_PLACEMENT_3D ( 'NONE', #6324, #14343, #12553 ) ;
#8072 = CARTESIAN_POINT ( 'NONE',  ( 2.873153789725825025, 3.954556930911862000, -13.46874999795161543 ) ) ;
#8073 = ORIENTED_EDGE ( 'NONE', *, *, #7528, .F. ) ;
#8074 = CARTESIAN_POINT ( 'NONE',  ( 16.28688694438835327, -7.664027248171309203, -32.00000000000000000 ) ) ;
#8075 = AXIS2_PLACEMENT_3D ( 'NONE', #17598, #4185, #7065 ) ;
#8076 = EDGE_CURVE ( 'NONE', #12765, #8963, #6413, .T. ) ;
#8077 = CARTESIAN_POINT ( 'NONE',  ( 11.84374999795161365, -4.888101187500000222, -3.383411828340740850E-14 ) ) ;
#8078 = EDGE_LOOP ( 'NONE', ( #15182, #13856 ) ) ;
#8079 = DIRECTION ( 'NONE',  ( 1.000000000000000000, 0.000000000000000000, 0.000000000000000000 ) ) ;
#8080 = CARTESIAN_POINT ( 'NONE',  ( 1.394999999999999574, -12.96210679857803960, 24.89775460606827551 ) ) ;
#8081 = CARTESIAN_POINT ( 'NONE',  ( -13.32184790671639618, 13.12143529358541549, 32.00000000000000000 ) ) ;
#8082 = DIRECTION ( 'NONE',  ( 0.000000000000000000, -6.870191984066573782E-16, -1.000000000000000000 ) ) ;
#8083 = CARTESIAN_POINT ( 'NONE',  ( -16.28688694438836038, -7.664027248171298545, -35.00000000000000000 ) ) ;
#8084 = ORIENTED_EDGE ( 'NONE', *, *, #11353, .T. ) ;
#8085 = CARTESIAN_POINT ( 'NONE',  ( 4.465502636338025688, -1.988169868018592412, -14.84374999795161543 ) ) ;
#8086 =( NAMED_UNIT ( * ) PLANE_ANGLE_UNIT ( ) SI_UNIT ( $, .RADIAN. ) );
#8087 = CARTESIAN_POINT ( 'NONE',  ( 90.56249999999998579, 0.000000000000000000, 3.796999999999998820 ) ) ;
#8088 = CIRCLE ( 'NONE', #10648, 1.000000000000000888 ) ;
#8089 = CARTESIAN_POINT ( 'NONE',  ( 5.700000000000001066, 0.000000000000000000, -13.97977757194595760 ) ) ;
#8090 = ORIENTED_EDGE ( 'NONE', *, *, #13212, .F. ) ;
#8091 = PRODUCT_DEFINITION ( 'UNKNOWN', '', #9895, #14204 ) ;
#8092 = CARTESIAN_POINT ( 'NONE',  ( 15.28688694438835505, -7.664027248171309203, 32.00000000000000000 ) ) ;
#8093 = DIRECTION ( 'NONE',  ( -1.000000000000000000, 0.000000000000000000, 0.000000000000000000 ) ) ;
#8094 = ADVANCED_FACE ( 'NONE', ( #10745 ), #18265, .T. ) ;
#8095 = CARTESIAN_POINT ( 'NONE',  ( 4.484949146646356688, -3.631840208645826351, -11.50000000000000355 ) ) ;
#8096 = LINE ( 'NONE', #12319, #12051 ) ;
#8097 = CARTESIAN_POINT ( 'NONE',  ( 2.000000000000001776, 0.000000000000000000, -7.800000000000000711 ) ) ;
#8098 = EDGE_LOOP ( 'NONE', ( #11464, #19061, #10051, #12656 ) ) ;
#8099 = DIRECTION ( 'NONE',  ( 1.000000000000000000, 1.224646799147353207E-16, 0.000000000000000000 ) ) ;
#8100 = COLOUR_RGB ( '', 0.31764706, 0.68627451, 0.89019608) ;
#8101 = DIRECTION ( 'NONE',  ( 0.000000000000000000, 0.000000000000000000, 1.000000000000000000 ) ) ;
#8102 = VERTEX_POINT ( 'NONE', #6610 ) ;
#8103 = EDGE_CURVE ( 'NONE', #5554, #16744, #18304, .T. ) ;
#8104 = CARTESIAN_POINT ( 'NONE',  ( 13.00000000000000533, 5.207209108562852684, -2.318398865532001363 ) ) ;
#8105 = ADVANCED_FACE ( 'NONE', ( #1738 ), #1927, .T. ) ;
#8106 = DIRECTION ( 'NONE',  ( 1.000000000000000000, 0.000000000000000000, 0.000000000000000000 ) ) ;
#8107 = ORIENTED_EDGE ( 'NONE', *, *, #12498, .F. ) ;
#8108 = CIRCLE ( 'NONE', #19283, 2.524999999999995914 ) ;
#8109 = EDGE_CURVE ( 'NONE', #10470, #3148, #9447, .T. ) ;
#8110 = CARTESIAN_POINT ( 'NONE',  ( 2.765633920072238183, -18.55949924794904504, 16.37294372382852004 ) ) ;
#8111 = CARTESIAN_POINT ( 'NONE',  ( 10.00000000000000533, -1.185096637661254171, 5.575441324182689229 ) ) ;
#8112 = EDGE_LOOP ( 'NONE', ( #4171, #15424, #3457, #14149 ) ) ;
#8113 = CIRCLE ( 'NONE', #4607, 28.06981291497571362 ) ;
#8114 = PLANE ( 'NONE',  #8510 ) ;
#8115 = CARTESIAN_POINT ( 'NONE',  ( 16.19790265903627358, 9.644882309621939598, 35.00000000000000000 ) ) ;
#8116 = CARTESIAN_POINT ( 'NONE',  ( -2.000000000000001776, 0.000000000000000000, 0.000000000000000000 ) ) ;
#8117 = ORIENTED_EDGE ( 'NONE', *, *, #5643, .T. ) ;
#8118 = FACE_OUTER_BOUND ( 'NONE', #3492, .T. ) ;
#8119 = ORIENTED_EDGE ( 'NONE', *, *, #12718, .F. ) ;
#8120 = EDGE_CURVE ( 'NONE', #19560, #15, #7925, .T. ) ;
#8121 = CARTESIAN_POINT ( 'NONE',  ( -34.92499999999994742, 0.000000000000000000, 7.500000000000000000 ) ) ;
#8122 = ORIENTED_EDGE ( 'NONE', *, *, #6407, .F. ) ;
#8123 = EDGE_CURVE ( 'NONE', #4347, #18719, #8171, .T. ) ;
#8124 = DIRECTION ( 'NONE',  ( 0.000000000000000000, 0.000000000000000000, -1.000000000000000000 ) ) ;
#8125 = AXIS2_PLACEMENT_3D ( 'NONE', #6825, #12951, #15284 ) ;
#8126 = CARTESIAN_POINT ( 'NONE',  ( -4.781284448697201483, -1.016293382781378485, -12.84374999795161543 ) ) ;
#8127 = DIRECTION ( 'NONE',  ( 1.000000000000000000, 0.000000000000000000, 0.000000000000000000 ) ) ;
#8128 = DIRECTION ( 'NONE',  ( 0.000000000000000000, 0.000000000000000000, -1.000000000000000000 ) ) ;
#8129 = ORIENTED_EDGE ( 'NONE', *, *, #1955, .T. ) ;
#8130 = DIRECTION ( 'NONE',  ( 1.000000000000000000, 0.000000000000000000, 0.000000000000000000 ) ) ;
#8131 = CARTESIAN_POINT ( 'NONE',  ( 16.28688694438835327, -7.664027248171309203, 32.00000000000000000 ) ) ;
#8132 = AXIS2_PLACEMENT_3D ( 'NONE', #14351, #17647, #8544 ) ;
#8133 = EDGE_LOOP ( 'NONE', ( #16008, #6280 ) ) ;
#8134 = DIRECTION ( 'NONE',  ( 1.000000000000000000, 0.000000000000000000, 0.000000000000000000 ) ) ;
#8135 = AXIS2_PLACEMENT_3D ( 'NONE', #5212, #9632, #14120 ) ;
#8136 = EDGE_CURVE ( 'NONE', #17840, #13931, #12558, .T. ) ;
#8137 = DIRECTION ( 'NONE',  ( 1.000000000000000000, 0.000000000000000000, 0.000000000000000000 ) ) ;
#8138 = DIRECTION ( 'NONE',  ( -1.000000000000000000, -6.419766481290788001E-33, -0.000000000000000000 ) ) ;
#8139 = ORIENTED_EDGE ( 'NONE', *, *, #3108, .F. ) ;
#8140 = CARTESIAN_POINT ( 'NONE',  ( 12.50000000000000533, -0.3020334839682081163, -5.763142191869158992 ) ) ;
#8141 = CARTESIAN_POINT ( 'NONE',  ( 7.312499995903225525, -4.936344801571268093, -2.850000000000058265 ) ) ;
#8142 = DIRECTION ( 'NONE',  ( 0.000000000000000000, 0.000000000000000000, -1.000000000000000000 ) ) ;
#8143 = VERTEX_POINT ( 'NONE', #3434 ) ;
#8144 = CARTESIAN_POINT ( 'NONE',  ( 13.00000000000000533, 0.2990843904630375860, -5.438532396800193958 ) ) ;
#8145 = EDGE_CURVE ( 'NONE', #3050, #5656, #18660, .T. ) ;
#8146 = CIRCLE ( 'NONE', #10706, 1.000000000000000888 ) ;
#8147 = ORIENTED_EDGE ( 'NONE', *, *, #13095, .F. ) ;
#8148 = SHAPE_DEFINITION_REPRESENTATION ( #1082, #15643 ) ;
#8149 = CARTESIAN_POINT ( 'NONE',  ( 0.000000000000000000, -15.74360496233395956, 18.28042085475273026 ) ) ;
#8150 = ADVANCED_FACE ( 'NONE', ( #15742 ), #16950, .T. ) ;
#8151 = DIRECTION ( 'NONE',  ( -1.000000000000000000, 0.000000000000000000, 0.000000000000000000 ) ) ;
#8152 = ORIENTED_EDGE ( 'NONE', *, *, #527, .T. ) ;
#8153 = ORIENTED_EDGE ( 'NONE', *, *, #5992, .F. ) ;
#8154 = CARTESIAN_POINT ( 'NONE',  ( -36.00000000000000000, -5.000000000000000888, -2.000000000000000000 ) ) ;
#8155 = CARTESIAN_POINT ( 'NONE',  ( 8.468749997951615427, 1.988169868018562436, 4.465502636338039011 ) ) ;
#8156 = VERTEX_POINT ( 'NONE', #3729 ) ;
#8157 = EDGE_CURVE ( 'NONE', #7944, #19214, #12715, .T. ) ;
#8158 = LINE ( 'NONE', #5351, #3273 ) ;
#8159 = CIRCLE ( 'NONE', #13903, 1.000000000000004441 ) ;
#8160 = EDGE_LOOP ( 'NONE', ( #2637, #18948, #468, #16573 ) ) ;
#8161 = CIRCLE ( 'NONE', #11672, 1.000000000000004441 ) ;
#8162 = LINE ( 'NONE', #262, #4767 ) ;
#8163 = CARTESIAN_POINT ( 'NONE',  ( -15.00000000000000355, 0.000000000000000000, 0.000000000000000000 ) ) ;
#8164 = FACE_BOUND ( 'NONE', #5742, .T. ) ;
#8165 = EDGE_LOOP ( 'NONE', ( #12609, #5224 ) ) ;
#8166 = DIRECTION ( 'NONE',  ( -1.000000000000000000, 0.000000000000000000, 0.000000000000000000 ) ) ;
#8167 = DIRECTION ( 'NONE',  ( 1.000000000000000000, 0.000000000000000000, 0.000000000000000000 ) ) ;
#8168 = ADVANCED_FACE ( 'NONE', ( #9850 ), #2511, .T. ) ;
#8169 = ORIENTED_EDGE ( 'NONE', *, *, #12035, .T. ) ;
#8170 = ORIENTED_EDGE ( 'NONE', *, *, #12460, .T. ) ;
#8171 = B_SPLINE_CURVE_WITH_KNOTS ( 'NONE', 3,
 ( #331, #12643, #12347, #6410, #18440, #4636 ),
 .UNSPECIFIED., .F., .F.,
 ( 4, 2, 4 ),
 ( 0.0004963285629696456008, 0.002127826186449799806, 0.003759323809929954012 ),
 .UNSPECIFIED. ) ;
#8172 = DIRECTION ( 'NONE',  ( -1.000000000000000000, -6.419766481290786633E-33, 0.000000000000000000 ) ) ;
#8173 = TOROIDAL_SURFACE ( 'NONE', #15849, 24.12539914357697768, 8.000000000000000000 ) ;
#8174 = AXIS2_PLACEMENT_3D ( 'NONE', #3773, #584, #967 ) ;
#8175 = CARTESIAN_POINT ( 'NONE',  ( 1.394999999999999574, 12.96210679857786552, 24.89775460606837143 ) ) ;
#8176 = FACE_OUTER_BOUND ( 'NONE', #1099, .T. ) ;
#8177 = ORIENTED_EDGE ( 'NONE', *, *, #10519, .F. ) ;
#8178 = CARTESIAN_POINT ( 'NONE',  ( 12.84374999795161543, 3.632567103900569361, -3.270778111535288080 ) ) ;
#8179 = CARTESIAN_POINT ( 'NONE',  ( -5.435144416706554624E-16, -9.514945144208892813, 22.37986894186668962 ) ) ;
#8180 = VERTEX_POINT ( 'NONE', #927 ) ;
#8181 = DIRECTION ( 'NONE',  ( -4.163336342344335449E-15, 1.000000000000000000, 0.000000000000000000 ) ) ;
#8182 = EDGE_CURVE ( 'NONE', #13666, #16380, #412, .T. ) ;
#8183 = EDGE_CURVE ( 'NONE', #15108, #12385, #11590, .T. ) ;
#8184 = DIRECTION ( 'NONE',  ( -1.000000000000000000, -1.224646799147353207E-16, 0.000000000000000000 ) ) ;
#8185 = AXIS2_PLACEMENT_3D ( 'NONE', #5516, #13319, #19420 ) ;
#8186 = CARTESIAN_POINT ( 'NONE',  ( -10.58013454126452224, -14.56230589874905235, -32.00000000000000000 ) ) ;
#8187 = CARTESIAN_POINT ( 'NONE',  ( -8.671566133830875600, 15.77352024078954429, -32.00000000000000000 ) ) ;
#8188 = LINE ( 'NONE', #694, #13309 ) ;
#8189 = CARTESIAN_POINT ( 'NONE',  ( 1.039999999999996705, 19.67366047555530173, 20.02152543075352398 ) ) ;
#8190 = EDGE_CURVE ( 'NONE', #9359, #7686, #14126, .T. ) ;
#8191 = EDGE_CURVE ( 'NONE', #17466, #11664, #16708, .T. ) ;
#8192 = CARTESIAN_POINT ( 'NONE',  ( 4.936344801571308061, 2.849999999999989875, -12.31249999590322552 ) ) ;
#8193 = ORIENTED_EDGE ( 'NONE', *, *, #16891, .T. ) ;
#8194 = CARTESIAN_POINT ( 'NONE',  ( -20.63749999999999929, 0.000000000000000000, 0.000000000000000000 ) ) ;
#8195 = DIRECTION ( 'NONE',  ( 1.000000000000000000, 0.000000000000000000, 0.000000000000000000 ) ) ;
#8196 = VECTOR ( 'NONE', #11021, 999.9999999999998863 ) ;
#8197 = PRODUCT_DEFINITION_CONTEXT ( 'detailed design', #13155, 'design' ) ;
#8198 = DIRECTION ( 'NONE',  ( 1.000000000000000000, 0.000000000000000000, 0.000000000000000000 ) ) ;
#8199 = DIRECTION ( 'NONE',  ( 0.000000000000000000, 0.000000000000000000, -1.000000000000000000 ) ) ;
#8200 = LINE ( 'NONE', #11107, #1244 ) ;
#8201 = VERTEX_POINT ( 'NONE', #2324 ) ;
#8202 = CARTESIAN_POINT ( 'NONE',  ( 0.7592463977762147209, -4.828194074574546413, 27.14986936243572657 ) ) ;
#8203 = AXIS2_PLACEMENT_3D ( 'NONE', #11907, #2593, #1202 ) ;
#8204 = CARTESIAN_POINT ( 'NONE',  ( 1.000000000000003331, 18.00000000000000355, 32.00000000000000000 ) ) ;
#8205 = ORIENTED_EDGE ( 'NONE', *, *, #11604, .F. ) ;
#8206 = CARTESIAN_POINT ( 'NONE',  ( 7.343749997951615427, -0.7741991708319229115, 4.888101187499994893 ) ) ;
#8207 = DIRECTION ( 'NONE',  ( 0.000000000000000000, 0.000000000000000000, 1.000000000000000000 ) ) ;
#8208 = EDGE_LOOP ( 'NONE', ( #14307, #6238 ) ) ;
#8209 = CARTESIAN_POINT ( 'NONE',  ( 0.006931069955678739909, -16.17493693894892104, 18.43696893154752914 ) ) ;
#8210 = CARTESIAN_POINT ( 'NONE',  ( 7.078124996927420476, 4.584782303107598267, -2.647025296874989664 ) ) ;
#8211 = CARTESIAN_POINT ( 'NONE',  ( 12.00000000000000533, -4.235925505221167064, 3.814044456245474279 ) ) ;
#8212 =( BOUNDED_SURFACE ( )  B_SPLINE_SURFACE ( 1, 2, ( 
 ( #15102, #16506, #10599, #15202, #4197, #16604, #4295, #11899, #8698, #16704, #4488, #7580, #13394, #10310, #13597, #15002, #19295 ),
 ( #11800, #1293, #18012, #2988, #2784, #13297, #5780, #9102, #19397, #1399, #5979, #1494, #2884, #8999, #7372, #5587, #8899 ) ),
 .UNSPECIFIED., .F., .F., .F. ) 
 B_SPLINE_SURFACE_WITH_KNOTS ( ( 2, 2 ),
 ( 3, 2, 2, 2, 2, 2, 2, 2, 3 ),
 ( 0.000000000000000000, 1.000000000000000000 ),
 ( 0.000000000000000000, 0.05000000000000000278, 0.1000000000000000056, 0.1499999999999999944, 0.2000000000000000111, 0.2500000000000000000, 0.2999999999999999889, 0.3499999999999999778, 0.4000000000000000222 ),
 .UNSPECIFIED. ) 
 GEOMETRIC_REPRESENTATION_ITEM ( )  RATIONAL_B_SPLINE_SURFACE ( (
 ( 1.000000000000000000, 0.9876883405951377704, 1.000000000000000000, 0.9876883405951377704, 1.000000000000000000, 0.9876883405951377704, 1.000000000000000000, 0.9876883405951377704, 1.000000000000000000, 0.9876883405951377704, 1.000000000000000000, 0.9876883405951377704, 1.000000000000000000, 0.9876883405951377704, 1.000000000000000000, 0.9876883405951377704, 1.000000000000000000),
 ( 1.000000000000000000, 0.9876883405951377704, 1.000000000000000000, 0.9876883405951377704, 1.000000000000000000, 0.9876883405951377704, 1.000000000000000000, 0.9876883405951377704, 1.000000000000000000, 0.9876883405951377704, 1.000000000000000000, 0.9876883405951377704, 1.000000000000000000, 0.9876883405951377704, 1.000000000000000000, 0.9876883405951377704, 1.000000000000000000) ) ) 
 REPRESENTATION_ITEM ( '' )  SURFACE ( )  );
#8213 = ORIENTED_EDGE ( 'NONE', *, *, #5731, .T. ) ;
#8214 = CIRCLE ( 'NONE', #15891, 1.000000000000003109 ) ;
#8215 = DIRECTION ( 'NONE',  ( 0.000000000000000000, 0.000000000000000000, 1.000000000000000000 ) ) ;
#8216 = CARTESIAN_POINT ( 'NONE',  ( -4.484949146646330931, 3.631840208645857437, -12.81249999590322552 ) ) ;
#8217 = FACE_BOUND ( 'NONE', #19173, .T. ) ;
#8218 = CIRCLE ( 'NONE', #4061, 1.000000000000003109 ) ;
#8219 = ADVANCED_FACE ( 'NONE', ( #2127, #3628, #837, #738, #1014, #17730, #12740, #5419, #15841, #8231, #17339, #636, #7005, #6814, #5325, #8530, #13129, #9750, #8329, #6713, #13035, #4023, #19220, #11528, #14439, #19035, #12835 ), #18933, .F. ) ;
#8220 = EDGE_LOOP ( 'NONE', ( #9158, #12419, #3774, #18379, #2346, #13879 ) ) ;
#8221 = CARTESIAN_POINT ( 'NONE',  ( -12.00000000000000178, 0.000000000000000000, 29.00000000000000355 ) ) ;
#8222 = ORIENTED_EDGE ( 'NONE', *, *, #13174, .F. ) ;
#8223 = ADVANCED_FACE ( 'NONE', ( #17442 ), #805, .T. ) ;
#8224 = DIRECTION ( 'NONE',  ( 1.000000000000000000, 0.000000000000000000, 0.000000000000000000 ) ) ;
#8225 = VERTEX_POINT ( 'NONE', #11922 ) ;
#8226 = CARTESIAN_POINT ( 'NONE',  ( 0.5279272304333944010, -11.57956866523235462, 24.43806413951671530 ) ) ;
#8227 = CARTESIAN_POINT ( 'NONE',  ( 0.02436607992776541887, 12.59161484032942901, -21.30679549418617924 ) ) ;
#8228 = CARTESIAN_POINT ( 'NONE',  ( 7.671566133830872047, 15.77352024078954784, 32.00000000000000000 ) ) ;
#8229 = CARTESIAN_POINT ( 'NONE',  ( -0.8944271909999155223, 6.368163355566236381E-16, 5.200000000000000178 ) ) ;
#8230 = EDGE_LOOP ( 'NONE', ( #18111, #15419, #666, #14770 ) ) ;
#8231 = FACE_BOUND ( 'NONE', #10018, .T. ) ;
#8232 = ADVANCED_FACE ( 'NONE', ( #19513 ), #16622, .T. ) ;
#8233 = DIRECTION ( 'NONE',  ( -1.000000000000000000, -0.000000000000000000, -0.000000000000000000 ) ) ;
#8234 = ORIENTED_EDGE ( 'NONE', *, *, #4935, .T. ) ;
#8235 = VECTOR ( 'NONE', #8257, 1000.000000000000000 ) ;
#8237 = EDGE_CURVE ( 'NONE', #9816, #18407, #8626, .T. ) ;
#8236 = EDGE_CURVE ( 'NONE', #7464, #7908, #9662, .T. ) ;
#8238 = DIRECTION ( 'NONE',  ( 0.000000000000000000, 0.000000000000000000, -1.000000000000000000 ) ) ;
#8239 = CARTESIAN_POINT ( 'NONE',  ( 0.000000000000000000, 0.000000000000000000, 4.000000000000000000 ) ) ;
#8240 = ORIENTED_EDGE ( 'NONE', *, *, #14921, .F. ) ;
#8241 = DIRECTION ( 'NONE',  ( -1.000000000000000000, 0.000000000000000000, 0.000000000000000000 ) ) ;
#8242 = CARTESIAN_POINT ( 'NONE',  ( 4.409619785863891472, -2.246813503491864150, -7.968749997951616315 ) ) ;
#8243 = CARTESIAN_POINT ( 'NONE',  ( 13.00000000000000178, -0.3329550909586923013, -4.877148943244129953 ) ) ;
#8244 = ORIENTED_EDGE ( 'NONE', *, *, #9382, .T. ) ;
#8245 = CARTESIAN_POINT ( 'NONE',  ( -12.32184790671639085, 13.12143529358541549, -35.00000000000000000 ) ) ;
#8246 = AXIS2_PLACEMENT_3D ( 'NONE', #3074, #7866, #3270 ) ;
#8247 = ORIENTED_EDGE ( 'NONE', *, *, #13583, .F. ) ;
#8248 = CONTEXT_DEPENDENT_SHAPE_REPRESENTATION ( #807, #16260 ) ;
#8249 =( NAMED_UNIT ( * ) SI_UNIT ( $, .STERADIAN. ) SOLID_ANGLE_UNIT ( ) );
#8250 = AXIS2_PLACEMENT_3D ( 'NONE', #9445, #18634, #12542 ) ;
#8251 = CARTESIAN_POINT ( 'NONE',  ( 7.343749997951615427, 4.620319390059829168, -1.773574444220725077 ) ) ;
#8252 = ORIENTED_EDGE ( 'NONE', *, *, #7556, .F. ) ;
#8253 = EDGE_LOOP ( 'NONE', ( #18383, #5821, #8985, #5405 ) ) ;
#8254 = DIRECTION ( 'NONE',  ( 1.000000000000000000, 0.000000000000000000, 0.000000000000000000 ) ) ;
#8255 = CARTESIAN_POINT ( 'NONE',  ( 6.500000000000005329, 4.484949146646356688, 3.631840208645826795 ) ) ;
#8256 = B_SPLINE_CURVE_WITH_KNOTS ( 'NONE', 3,
 ( #4549, #5845, #16468, #1455 ),
 .UNSPECIFIED., .F., .F.,
 ( 4, 4 ),
 ( 0.005258120783916788929, 0.005948386350302939385 ),
 .UNSPECIFIED. ) ;
#8257 = DIRECTION ( 'NONE',  ( -1.000000000000000000, -0.000000000000000000, 0.000000000000000000 ) ) ;
#8258 = ORIENTED_EDGE ( 'NONE', *, *, #3767, .F. ) ;
#8259 = CARTESIAN_POINT ( 'NONE',  ( -4.233219804643852946, 2.444050593750049405, -11.84374999795161365 ) ) ;
#8260 = PRODUCT ( 'radial cylindrical roller bearing_iso_ISO 15 RCR - 3712 - 24,SI,NC,24', 'radial cylindrical roller bearing_iso_ISO 15 RCR - 3712 - 24,SI,NC,24', '', ( #13860 ) ) ;
#8261 = CIRCLE ( 'NONE', #4428, 24.12539914357697413 ) ;
#8262 = EDGE_LOOP ( 'NONE', ( #8476, #11822 ) ) ;
#8263 = CARTESIAN_POINT ( 'NONE',  ( -2.000000000000001776, 4.898587196589412829E-16, -4.000000000000000000 ) ) ;
#8264 = CARTESIAN_POINT ( 'NONE',  ( -4.366025403784388637, -7.562177826491097044, 37.99999999999999289 ) ) ;
#8265 = CARTESIAN_POINT ( 'NONE',  ( 2.718184757033984766, -16.91181672897746324, 18.89296398180185932 ) ) ;
#8266 = ORIENTED_EDGE ( 'NONE', *, *, #259, .T. ) ;
#8267 = DIRECTION ( 'NONE',  ( -1.000000000000000000, -6.419766481290786633E-33, 0.000000000000000000 ) ) ;
#8268 =( LENGTH_UNIT ( ) NAMED_UNIT ( * ) SI_UNIT ( .MILLI., .METRE. ) );
#8269 = DIRECTION ( 'NONE',  ( -0.4330127018922130255, 0.7500000000000049960, 0.4999999999999980571 ) ) ;
#8270 = ORIENTED_EDGE ( 'NONE', *, *, #15378, .F. ) ;
#8271 = ORIENTED_EDGE ( 'NONE', *, *, #9164, .T. ) ;
#8272 = CARTESIAN_POINT ( 'NONE',  ( -4.840010801796527318, -3.143139765844555900, -7.500000000000005329 ) ) ;
#8273 = CIRCLE ( 'NONE', #11784, 6.735000000000022524 ) ;
#8274 = CARTESIAN_POINT ( 'NONE',  ( -1.799999999999999600, 4.898587196589412829E-16, 4.000000000000000000 ) ) ;
#8275 = DIRECTION ( 'NONE',  ( -1.000000000000000000, 0.000000000000000000, 0.000000000000000000 ) ) ;
#8276 =( GEOMETRIC_REPRESENTATION_CONTEXT ( 3 ) GLOBAL_UNCERTAINTY_ASSIGNED_CONTEXT ( ( #16594 ) ) GLOBAL_UNIT_ASSIGNED_CONTEXT ( ( #10079, #13168, #14375 ) ) REPRESENTATION_CONTEXT ( 'NONE', 'WORKASPACE' ) );
#8277 = VERTEX_POINT ( 'NONE', #1419 ) ;
#8278 = CARTESIAN_POINT ( 'NONE',  ( -8.671566133830875600, 15.77352024078954429, 32.00000000000000000 ) ) ;
#8279 = DIRECTION ( 'NONE',  ( 0.000000000000000000, 0.000000000000000000, 1.000000000000000000 ) ) ;
#8280 = EDGE_LOOP ( 'NONE', ( #15169, #2560, #375, #4654, #14592, #16995 ) ) ;
#8281 = CARTESIAN_POINT ( 'NONE',  ( 18.96448111170889206, 1.130229351527639148, 35.00000000000000000 ) ) ;
#8282 = ADVANCED_FACE ( 'NONE', ( #8821 ), #2902, .T. ) ;
#8283 = CARTESIAN_POINT ( 'NONE',  ( 13.00000000000000533, 4.611396867937201272, 3.350375938067096548 ) ) ;
#8284 = AXIS2_PLACEMENT_3D ( 'NONE', #5925, #16643, #12244 ) ;
#8285 = DIRECTION ( 'NONE',  ( 0.000000000000000000, 0.000000000000000000, 1.000000000000000000 ) ) ;
#8286 = DIRECTION ( 'NONE',  ( 0.000000000000000000, 0.000000000000000000, 1.000000000000000000 ) ) ;
#8287 = CARTESIAN_POINT ( 'NONE',  ( -3.350375938067128967, -4.611396867937178179, -13.00000000000000533 ) ) ;
#8288 = DIRECTION ( 'NONE',  ( 1.000000000000000000, 3.873737557103174326E-15, 0.000000000000000000 ) ) ;
#8289 = SURFACE_STYLE_FILL_AREA ( #2185 ) ;
#8290 = DIRECTION ( 'NONE',  ( -1.000000000000000000, -0.000000000000000000, -0.000000000000000000 ) ) ;
#8291 = PRODUCT_DEFINITION_FORMATION_WITH_SPECIFIED_SOURCE ( 'ANY', '', #2506, .NOT_KNOWN. ) ;
#8292 = CARTESIAN_POINT ( 'NONE',  ( 2.299999999999998490, 0.000000000000000000, -8.800000000000023803 ) ) ;
#8293 = ORIENTED_EDGE ( 'NONE', *, *, #15204, .F. ) ;
#8294 = CARTESIAN_POINT ( 'NONE',  ( 0.006974771092478172958, -9.686319561460797090, -22.53337530003413747 ) ) ;
#8295 = DIRECTION ( 'NONE',  ( 0.000000000000000000, 0.000000000000000000, 1.000000000000000000 ) ) ;
#8296 = CARTESIAN_POINT ( 'NONE',  ( 2.695436003842704764, -4.150607464521812062, -13.34374999795161365 ) ) ;
#8297 = CARTESIAN_POINT ( 'NONE',  ( 11.84374999795161365, -2.444050593749961031, -4.233219804643904460 ) ) ;
#8298 = ADVANCED_FACE ( 'NONE', ( #10334 ), #13318, .F. ) ;
#8299 = ORIENTED_EDGE ( 'NONE', *, *, #162, .T. ) ;
#8300 = CARTESIAN_POINT ( 'NONE',  ( -0.5745956068256975469, 5.466912017135477697, -14.11718749948790830 ) ) ;
#8301 = CARTESIAN_POINT ( 'NONE',  ( -0.5109457054262123155, -4.861323657744403448, -8.843749997951615427 ) ) ;
#8302 = ORIENTED_EDGE ( 'NONE', *, *, #8120, .F. ) ;
#8303 = CARTESIAN_POINT ( 'NONE',  ( 14.34374999795161365, -3.499494075959791672, -3.499494075959840078 ) ) ;
#8304 = DIRECTION ( 'NONE',  ( -0.000000000000000000, -0.000000000000000000, -1.000000000000000000 ) ) ;
#8305 = PRESENTATION_LAYER_ASSIGNMENT (  '', '', ( #12465 ) ) ;
#8306 = ORIENTED_EDGE ( 'NONE', *, *, #399, .T. ) ;
#8307 = CYLINDRICAL_SURFACE ( 'NONE', #17090, 1.000000000000002665 ) ;
#8308 = AXIS2_PLACEMENT_3D ( 'NONE', #4331, #16542, #5817 ) ;
#8309 = EDGE_CURVE ( 'NONE', #4750, #5566, #17317, .T. ) ;
#8310 = CARTESIAN_POINT ( 'NONE',  ( 0.000000000000000000, 0.000000000000000000, 29.00000000000000355 ) ) ;
#8311 = DIRECTION ( 'NONE',  ( 0.000000000000000000, 0.000000000000000000, 1.000000000000000000 ) ) ;
#8312 = CARTESIAN_POINT ( 'NONE',  ( 0.000000000000000000, 0.000000000000000000, 0.000000000000000000 ) ) ;
#8313 = VERTEX_POINT ( 'NONE', #18126 ) ;
#8314 = CARTESIAN_POINT ( 'NONE',  ( 1.749999999999998002, -27.68468304288255766, -4.633866840649213614 ) ) ;
#8315 = CARTESIAN_POINT ( 'NONE',  ( 3.499494075959815653, 3.499494075959816541, -13.96874999795161365 ) ) ;
#8316 = EDGE_LOOP ( 'NONE', ( #5315, #586, #7766, #15534 ) ) ;
#8317 = LINE ( 'NONE', #2498, #15021 ) ;
#8318 = ORIENTED_EDGE ( 'NONE', *, *, #4079, .T. ) ;
#8319 = CARTESIAN_POINT ( 'NONE',  ( 13.00000000000000000, 1.727010089215937905, 5.432074755721460591 ) ) ;
#8320 = VERTEX_POINT ( 'NONE', #10621 ) ;
#8321 = CIRCLE ( 'NONE', #12169, 6.760799999999997034 ) ;
#8322 = VECTOR ( 'NONE', #6088, 1000.000000000000000 ) ;
#8323 = CARTESIAN_POINT ( 'NONE',  ( -2.300000000000000711, 0.000000000000000000, -6.200000000000020606 ) ) ;
#8324 = DIRECTION ( 'NONE',  ( 0.000000000000000000, 0.000000000000000000, 1.000000000000000000 ) ) ;
#8325 = ADVANCED_FACE ( 'NONE', ( #7294 ), #10387, .F. ) ;
#8326 = PLANE ( 'NONE',  #11890 ) ;
#8327 = CARTESIAN_POINT ( 'NONE',  ( -6.626241948324210540, -16.73597674598852336, -32.00000000000000000 ) ) ;
#8328 = ORIENTED_EDGE ( 'NONE', *, *, #10326, .F. ) ;
#8329 = FACE_BOUND ( 'NONE', #13929, .T. ) ;
#8330 = CARTESIAN_POINT ( 'NONE',  ( 2.789999999999999147, -23.17675759782035172, -7.772527002114682837 ) ) ;
#8331 = EDGE_CURVE ( 'NONE', #17936, #15544, #9975, .T. ) ;
#8332 = ORIENTED_EDGE ( 'NONE', *, *, #879, .F. ) ;
#8333 =( BOUNDED_CURVE ( )  B_SPLINE_CURVE ( 2, ( #16503, #4391, #10503, #2781, #14999, #8897, #8996, #1291, #16601, #15100, #1396, #7476, #13595, #19693, #5977, #12100, #15198 ),
 .UNSPECIFIED., .F., .F. ) 
 B_SPLINE_CURVE_WITH_KNOTS ( ( 3, 2, 2, 2, 2, 2, 2, 2, 3 ),
 ( 0.000000000000000000, 0.05000000000000000971, 0.1000000000000000194, 0.1499999999999999944, 0.2000000000000000389, 0.2500000000000000000, 0.2999999999999999889, 0.3499999999999999223, 0.4000000000000000777 ),
 .UNSPECIFIED. ) 
 CURVE ( )  GEOMETRIC_REPRESENTATION_ITEM ( )  RATIONAL_B_SPLINE_CURVE ( ( 1.000000000000000000, 0.9876883405951377704, 1.000000000000000000, 0.9876883405951377704, 1.000000000000000000, 0.9876883405951377704, 1.000000000000000000, 0.9876883405951377704, 1.000000000000000000, 0.9876883405951377704, 1.000000000000000000, 0.9876883405951377704, 1.000000000000000000, 0.9876883405951377704, 1.000000000000000000, 0.9876883405951377704, 1.000000000000000000 ) ) 
 REPRESENTATION_ITEM ( '' )  );
#8334 = ADVANCED_FACE ( 'NONE', ( #113 ), #15520, .T. ) ;
#8335 = CIRCLE ( 'NONE', #8657, 24.12539914357697413 ) ;
#8336 = DIRECTION ( 'NONE',  ( 0.000000000000000000, 0.000000000000000000, -1.000000000000000000 ) ) ;
#8337 = LINE ( 'NONE', #4837, #1957 ) ;
#8338 = CARTESIAN_POINT ( 'NONE',  ( -4.780397808154247308, 1.280903732194486722, -13.96874999795161365 ) ) ;
#8339 = EDGE_LOOP ( 'NONE', ( #10831, #8922, #12824, #12446 ) ) ;
#8340 = DIRECTION ( 'NONE',  ( 0.000000000000000000, 0.000000000000000000, -1.000000000000000000 ) ) ;
#8341 = DIRECTION ( 'NONE',  ( 0.5000000000000097700, 0.8660254037844329345, 0.000000000000000000 ) ) ;
#8342 = CARTESIAN_POINT ( 'NONE',  ( -5.209999999999999964, 0.000000000000000000, 0.000000000000000000 ) ) ;
#8343 = VERTEX_POINT ( 'NONE', #4910 ) ;
#8344 = EDGE_CURVE ( 'NONE', #18748, #7195, #63, .T. ) ;
#8345 = CARTESIAN_POINT ( 'NONE',  ( 0.000000000000000000, -8.000000000000003553, 37.99999999999999289 ) ) ;
#8346 = ORIENTED_EDGE ( 'NONE', *, *, #19101, .T. ) ;
#8347 = ITEM_DEFINED_TRANSFORMATION ( 'NONE', 'NONE', #15623,  #16724 ) ;
#8348 = CARTESIAN_POINT ( 'NONE',  ( 7.343749997951615427, 3.846120219227923798, 3.114526743279282694 ) ) ;
#8349 = DIRECTION ( 'NONE',  ( 0.000000000000000000, 0.000000000000000000, 1.000000000000000000 ) ) ;
#8350 = ORIENTED_EDGE ( 'NONE', *, *, #5422, .T. ) ;
#8351 = VERTEX_POINT ( 'NONE', #8001 ) ;
#8352 = CARTESIAN_POINT ( 'NONE',  ( 5.312660008432906977, -6.098169837403623283, -0.06756670027994693406 ) ) ;
#8353 = CARTESIAN_POINT ( 'NONE',  ( 4.465502636338025688, -1.988169868018592856, -14.46874999795161720 ) ) ;
#8354 = VECTOR ( 'NONE', #3634, 1000.000000000000000 ) ;
#8355 = CARTESIAN_POINT ( 'NONE',  ( 4.366025403784385972, 7.562177826491085497, 37.99999999999999289 ) ) ;
#8356 = EDGE_CURVE ( 'NONE', #17288, #2407, #7378, .T. ) ;
#8357 = EDGE_LOOP ( 'NONE', ( #18033, #19747, #7760, #7771 ) ) ;
#8358 = ADVANCED_FACE ( 'NONE', ( #4712 ), #1335, .T. ) ;
#8359 = AXIS2_PLACEMENT_3D ( 'NONE', #14749, #2246, #7121 ) ;
#8360 = DIRECTION ( 'NONE',  ( -1.000000000000000000, 0.000000000000000000, 0.000000000000000000 ) ) ;
#8361 = ORIENTED_EDGE ( 'NONE', *, *, #703, .F. ) ;
#8362 = B_SPLINE_CURVE_WITH_KNOTS ( 'NONE', 3,
 ( #15806, #10910, #18802, #14010 ),
 .UNSPECIFIED., .F., .F.,
 ( 4, 4 ),
 ( 0.000000000000000000, 0.001126652051248517921 ),
 .UNSPECIFIED. ) ;
#8363 = VECTOR ( 'NONE', #1812, 1000.000000000000000 ) ;
#8364 = CARTESIAN_POINT ( 'NONE',  ( 0.000000000000000000, 0.000000000000000000, -33.00000000000000000 ) ) ;
#8365 = EDGE_CURVE ( 'NONE', #2569, #16939, #12426, .T. ) ;
#8366 = EDGE_CURVE ( 'NONE', #9059, #18970, #10288, .T. ) ;
#8367 = AXIS2_PLACEMENT_3D ( 'NONE', #2218, #19217, #17629 ) ;
#8368 = CARTESIAN_POINT ( 'NONE',  ( -15.00000000000000355, 4.400000000000000355, 0.000000000000000000 ) ) ;
#8369 = CARTESIAN_POINT ( 'NONE',  ( -4.942249507334553371, 0.2590123213421660631, -10.34374999795161543 ) ) ;
#8370 = CARTESIAN_POINT ( 'NONE',  ( 0.000000000000000000, 0.000000000000000000, 0.000000000000000000 ) ) ;
#8371 = DIRECTION ( 'NONE',  ( 0.000000000000000000, 0.000000000000000000, 1.000000000000000000 ) ) ;
#8372 = ORIENTED_EDGE ( 'NONE', *, *, #8183, .T. ) ;
#8373 = ORIENTED_EDGE ( 'NONE', *, *, #12078, .T. ) ;
#8374 = CARTESIAN_POINT ( 'NONE',  ( -4.150607464521828938, -2.695436003842674566, -7.968749997951616315 ) ) ;
#8375 = EDGE_CURVE ( 'NONE', #6790, #619, #11212, .T. ) ;
#8376 = CARTESIAN_POINT ( 'NONE',  ( 13.00000000000000178, 3.947414994554159229, -2.883678330714892990 ) ) ;
#8377 = AXIS2_PLACEMENT_3D ( 'NONE', #19111, #5403, #16125 ) ;
#8378 = DIRECTION ( 'NONE',  ( -1.000000000000000000, -0.000000000000000000, 0.000000000000000000 ) ) ;
#8379 = AXIS2_PLACEMENT_3D ( 'NONE', #8774, #13080, #5463 ) ;
#8380 = ORIENTED_EDGE ( 'NONE', *, *, #4395, .T. ) ;
#8381 = CARTESIAN_POINT ( 'NONE',  ( 10.46874999795161720, 1.016293382781477961, -4.781284448697179279 ) ) ;
#8382 = AXIS2_PLACEMENT_3D ( 'NONE', #14308, #3503, #806 ) ;
#8383 = CARTESIAN_POINT ( 'NONE',  ( 13.00000000000000178, -4.416988234087956045, -2.093740232017208935 ) ) ;
#8384 = VERTEX_POINT ( 'NONE', #15715 ) ;
#8385 = CARTESIAN_POINT ( 'NONE',  ( -39.64101615137757761, -1.650388831904890594E-13, 37.99999999999999289 ) ) ;
#8386 = AXIS2_PLACEMENT_3D ( 'NONE', #17594, #17791, #3882 ) ;
#8387 = CARTESIAN_POINT ( 'NONE',  ( 6.500000000000005329, 0.9027913098498568933, -5.700000000000000178 ) ) ;
#8388 = CARTESIAN_POINT ( 'NONE',  ( 0.02436607992776151574, -18.55949924794880346, -16.37294372382878649 ) ) ;
#8389 = EDGE_CURVE ( 'NONE', #8962, #15303, #1652, .T. ) ;
#8390 = DIRECTION ( 'NONE',  ( 0.000000000000000000, 0.000000000000000000, 1.000000000000000000 ) ) ;
#8391 = DIRECTION ( 'NONE',  ( -0.000000000000000000, -0.000000000000000000, 1.000000000000000000 ) ) ;
#8392 = AXIS2_PLACEMENT_3D ( 'NONE', #11066, #15870, #8360 ) ;
#8393 = CARTESIAN_POINT ( 'NONE',  ( -18.68117051311639543, -3.372863662543042818, -32.00000000000000000 ) ) ;
#8394 = LINE ( 'NONE', #6869, #9996 ) ;
#8395 = VECTOR ( 'NONE', #8848, 1000.000000000000000 ) ;
#8396 = CARTESIAN_POINT ( 'NONE',  ( -2.849999999999989431, 4.936344801571308061, -7.312499995903225525 ) ) ;
#8397 = ORIENTED_EDGE ( 'NONE', *, *, #6001, .T. ) ;
#8398 = CARTESIAN_POINT ( 'NONE',  ( 13.00000000000000000, 1.727010089215937905, 5.432074755721460591 ) ) ;
#8399 = DIRECTION ( 'NONE',  ( 0.000000000000000000, 1.224646799147358384E-16, 1.000000000000000000 ) ) ;
#8400 = AXIS2_PLACEMENT_3D ( 'NONE', #641, #11442, #6716 ) ;
#8401 = UNCERTAINTY_MEASURE_WITH_UNIT (LENGTH_MEASURE( 1.000000000000000082E-05 ), #14963, 'distance_accuracy_value', 'NONE');
#8402 = DIRECTION ( 'NONE',  ( -0.000000000000000000, -0.000000000000000000, 1.000000000000000000 ) ) ;
#8403 = ADVANCED_FACE ( 'NONE', ( #19010 ), #16399, .F. ) ;
#8404 = VECTOR ( 'NONE', #6236, 1000.000000000000114 ) ;
#8405 = CARTESIAN_POINT ( 'NONE',  ( 6.968749997951614539, -4.620319390059841602, 1.773574444220693103 ) ) ;
#8406 = LINE ( 'NONE', #9818, #6138 ) ;
#8407 = CARTESIAN_POINT ( 'NONE',  ( -4.861323657744403448, 0.5109457054262118714, -13.84374999795161543 ) ) ;
#8408 = ORIENTED_EDGE ( 'NONE', *, *, #9103, .T. ) ;
#8409 = CARTESIAN_POINT ( 'NONE',  ( 12.34374999795161543, -4.888101187499994893, -0.7741991708319226895 ) ) ;
#8410 = CARTESIAN_POINT ( 'NONE',  ( 0.5321745326902588280, 26.83036154824994668, -3.467596033028380376 ) ) ;
#8411 = AXIS2_PLACEMENT_3D ( 'NONE', #7535, #11758, #14862 ) ;
#8412 = ORIENTED_EDGE ( 'NONE', *, *, #2920, .F. ) ;
#8413 = CARTESIAN_POINT ( 'NONE',  ( 2.789999999999999147, -24.63872515616084513, 2.336989772644183283 ) ) ;
#8414 = ADVANCED_FACE ( 'NONE', ( #6980 ), #14415, .T. ) ;
#8415 = DIRECTION ( 'NONE',  ( 0.000000000000000000, 0.000000000000000000, 1.000000000000000000 ) ) ;
#8416 = CIRCLE ( 'NONE', #19586, 28.06981291497571007 ) ;
#8417 = VECTOR ( 'NONE', #11498, 1000.000000000000000 ) ;
#8418 = DIRECTION ( 'NONE',  ( -0.000000000000000000, 1.000000000000000000, 1.224646799147353207E-16 ) ) ;
#8419 = CARTESIAN_POINT ( 'NONE',  ( 4.500000000000000000, 5.510910596163088569E-16, -33.00000000000000000 ) ) ;
#8420 = ORIENTED_EDGE ( 'NONE', *, *, #19645, .T. ) ;
#8421 = PLANE ( 'NONE',  #2119 ) ;
#8422 = PRESENTATION_STYLE_ASSIGNMENT (( #17522 ) ) ;
#8423 = DIRECTION ( 'NONE',  ( -1.000000000000000000, 0.000000000000000000, 0.000000000000000000 ) ) ;
#8424 = ORIENTED_EDGE ( 'NONE', *, *, #13948, .F. ) ;
#8425 = FACE_OUTER_BOUND ( 'NONE', #4734, .T. ) ;
#8426 = ORIENTED_EDGE ( 'NONE', *, *, #16149, .F. ) ;
#8427 = CARTESIAN_POINT ( 'NONE',  ( 7.312499995903225525, -4.936344801571327601, 2.849999999999954348 ) ) ;
#8428 = MECHANICAL_DESIGN_GEOMETRIC_PRESENTATION_REPRESENTATION (  '', ( #9723 ), #12267 ) ;
#8429 = VERTEX_POINT ( 'NONE', #11504 ) ;
#8430 = APPLICATION_CONTEXT ( 'automotive_design' ) ;
#8431 = CYLINDRICAL_SURFACE ( 'NONE', #9924, 1.000000000000004441 ) ;
#8432 = ADVANCED_FACE ( 'NONE', ( #3799 ), #17606, .F. ) ;
#8433 = CARTESIAN_POINT ( 'NONE',  ( -2.299999999999996270, 0.000000000000000000, -9.000000000000019540 ) ) ;
#8434 = PRODUCT_DEFINITION_SHAPE ( 'NONE', 'NONE',  #19784 ) ;
#8435 = CARTESIAN_POINT ( 'NONE',  ( 0.000000000000000000, 0.000000000000000000, 32.00000000000000000 ) ) ;
#8437 = DIRECTION ( 'NONE',  ( 1.000000000000000000, 1.224646799147353207E-16, -0.000000000000000000 ) ) ;
#8436 = B_SPLINE_CURVE_WITH_KNOTS ( 'NONE', 3,
 ( #12585, #6355, #16796, #4580, #13983, #3375 ),
 .UNSPECIFIED., .F., .F.,
 ( 4, 2, 4 ),
 ( 1.979325885420663486E-07, 0.001878588715165612974, 0.003756979497742683576 ),
 .UNSPECIFIED. ) ;
#8438 = VERTEX_POINT ( 'NONE', #3998 ) ;
#8439 = DIRECTION ( 'NONE',  ( 1.000000000000000000, 0.000000000000000000, 0.000000000000000000 ) ) ;
#8440 = DIRECTION ( 'NONE',  ( 1.000000000000000000, 0.000000000000000000, 0.000000000000000000 ) ) ;
#8441 = ORIENTED_EDGE ( 'NONE', *, *, #13612, .F. ) ;
#8442 = B_SPLINE_CURVE_WITH_KNOTS ( 'NONE', 3,
 ( #9220, #1608, #18226, #7601 ),
 .UNSPECIFIED., .F., .F.,
 ( 4, 4 ),
 ( 0.005258214619651957987, 0.005948481662034167325 ),
 .UNSPECIFIED. ) ;
#8443 = DIRECTION ( 'NONE',  ( 0.000000000000000000, 0.000000000000000000, 1.000000000000000000 ) ) ;
#8444 = EDGE_CURVE ( 'NONE', #11356, #17411, #13468, .T. ) ;
#8445 = FACE_OUTER_BOUND ( 'NONE', #12306, .T. ) ;
#8446 = EDGE_CURVE ( 'NONE', #9696, #9010, #17957, .T. ) ;
#8447 = VERTEX_POINT ( 'NONE', #4194 ) ;
#8448 = CARTESIAN_POINT ( 'NONE',  ( 6.843749997951615427, -4.233219804643852946, -2.444050593750049849 ) ) ;
#8449 = LINE ( 'NONE', #845, #14584 ) ;
#8450 = FACE_BOUND ( 'NONE', #8612, .T. ) ;
#8451 = AXIS2_PLACEMENT_3D ( 'NONE', #19, #10439, #12334 ) ;
#8452 = EDGE_LOOP ( 'NONE', ( #9073, #19432 ) ) ;
#8453 = PLANE ( 'NONE',  #469 ) ;
#8454 = ORIENTED_EDGE ( 'NONE', *, *, #8797, .F. ) ;
#8455 = CARTESIAN_POINT ( 'NONE',  ( 0.000000000000000000, 0.000000000000000000, 0.000000000000000000 ) ) ;
#8456 = CARTESIAN_POINT ( 'NONE',  ( 2.601776144743014996, -23.64332819722373813, -10.68696068830432466 ) ) ;
#8457 = EDGE_CURVE ( 'NONE', #1803, #8447, #6427, .T. ) ;
#8458 = CARTESIAN_POINT ( 'NONE',  ( -15.19790265903627180, 9.644882309621941374, -35.00000000000000000 ) ) ;
#8459 = ORIENTED_EDGE ( 'NONE', *, *, #9588, .T. ) ;
#8460 = CARTESIAN_POINT ( 'NONE',  ( 0.6180618139040615633, -23.93436800624301242, 12.96259772325168314 ) ) ;
#8461 = FACE_OUTER_BOUND ( 'NONE', #6735, .T. ) ;
#8462 = AXIS2_PLACEMENT_3D ( 'NONE', #14556, #14652, #3743 ) ;
#8463 = DIRECTION ( 'NONE',  ( 0.000000000000000000, 0.000000000000000000, -1.000000000000000000 ) ) ;
#8464 = ORIENTED_EDGE ( 'NONE', *, *, #14468, .F. ) ;
#8465 =( BOUNDED_CURVE ( )  B_SPLINE_CURVE ( 2, ( #18210, #1593, #9107, #15209, #13602, #4397, #4299, #7483, #5889, #1404, #15107, #12770, #1298, #1498, #19700 ),
 .UNSPECIFIED., .F., .F. ) 
 B_SPLINE_CURVE_WITH_KNOTS ( ( 3, 2, 2, 2, 2, 2, 2, 3 ),
 ( 0.000000000000000000, 0.05000000000000000278, 0.1000000000000000056, 0.1499999999999999944, 0.2000000000000000111, 0.2500000000000000000, 0.2999999999999999889, 0.3333180920165871863 ),
 .UNSPECIFIED. ) 
 CURVE ( )  GEOMETRIC_REPRESENTATION_ITEM ( )  RATIONAL_B_SPLINE_CURVE ( ( 1.000000000000000000, 0.9876883405951377704, 1.000000000000000000, 0.9876883405951377704, 1.000000000000000000, 0.9876883405951377704, 1.000000000000000000, 0.9876883405951377704, 1.000000000000000000, 0.9876883405951377704, 1.000000000000000000, 0.9876883405951377704, 1.000000000000000000, 0.9917959799814384247, 0.9945256517182510247 ) ) 
 REPRESENTATION_ITEM ( '' )  );
#8466 = CIRCLE ( 'NONE', #9745, 2.524999999999996358 ) ;
#8467 = ORIENTED_EDGE ( 'NONE', *, *, #7711, .T. ) ;
#8468 = MECHANICAL_DESIGN_GEOMETRIC_PRESENTATION_REPRESENTATION (  '', ( #11019 ), #18373 ) ;
#8469 = DIRECTION ( 'NONE',  ( 0.000000000000000000, 0.000000000000000000, -1.000000000000000000 ) ) ;
#8470 = DIRECTION ( 'NONE',  ( 0.000000000000000000, 0.000000000000000000, -1.000000000000000000 ) ) ;
#8471 = ORIENTED_EDGE ( 'NONE', *, *, #11689, .T. ) ;
#8472 = CARTESIAN_POINT ( 'NONE',  ( -4.233219804643852946, 2.444050593750049405, -11.46874999795161543 ) ) ;
#8473 = DIRECTION ( 'NONE',  ( 1.000000000000000000, 0.000000000000000000, 0.000000000000000000 ) ) ;
#8474 = CARTESIAN_POINT ( 'NONE',  ( 2.647025296874957689, -4.584782303107616031, -7.078124996927420476 ) ) ;
#8475 = EDGE_CURVE ( 'NONE', #1120, #14880, #11797, .T. ) ;
#8476 = ORIENTED_EDGE ( 'NONE', *, *, #2287, .F. ) ;
#8477 = VERTEX_POINT ( 'NONE', #13391 ) ;
#8478 = EDGE_CURVE ( 'NONE', #5711, #18074, #17636, .T. ) ;
#8479 = CARTESIAN_POINT ( 'NONE',  ( -90.00000000000000000, 7.347880794884145374E-16, 6.000000000000021316 ) ) ;
#8480 = CARTESIAN_POINT ( 'NONE',  ( 5.626241948324195441, -16.73597674598852691, 32.00000000000000000 ) ) ;
#8481 = CIRCLE ( 'NONE', #19653, 1.000000000000000888 ) ;
#8482 = CARTESIAN_POINT ( 'NONE',  ( -2.068159791354182708, 5.387740456496234565, -6.500000000000005329 ) ) ;
#8483 = AXIS2_PLACEMENT_3D ( 'NONE', #13137, #3933, #10052 ) ;
#8484 = ORIENTED_EDGE ( 'NONE', *, *, #11969, .T. ) ;
#8485 = CARTESIAN_POINT ( 'NONE',  ( 13.96874999795161365, 4.780397808154273065, -1.280903732194386802 ) ) ;
#8486 = EDGE_CURVE ( 'NONE', #2766, #12340, #11505, .T. ) ;
#8487 = CARTESIAN_POINT ( 'NONE',  ( 11.81249999590322552, 2.068159791354258648, -5.387740456496205255 ) ) ;
#8488 = EDGE_LOOP ( 'NONE', ( #1330, #10081, #19024, #14617 ) ) ;
#8489 = CARTESIAN_POINT ( 'NONE',  ( 4.999999999999963585, 7.196152422706642682, 37.99999999999999289 ) ) ;
#8490 = EDGE_CURVE ( 'NONE', #12340, #15059, #5584, .T. ) ;
#8491 = DIRECTION ( 'NONE',  ( 1.000000000000000000, 0.000000000000000000, 0.000000000000000000 ) ) ;
#8492 = CYLINDRICAL_SURFACE ( 'NONE', #6508, 9.500000000000000000 ) ;
#8493 = DIRECTION ( 'NONE',  ( 1.000000000000000000, 0.000000000000000000, 0.000000000000000000 ) ) ;
#8494 = AXIS2_PLACEMENT_3D ( 'NONE', #9056, #18356, #9254 ) ;
#8495 = CARTESIAN_POINT ( 'NONE',  ( 10.64522241986047568, 2.725425358843983450E-16, 5.700000000000002842 ) ) ;
#8496 = FILL_AREA_STYLE ('',( #10001 ) ) ;
#8497 = DIRECTION ( 'NONE',  ( -1.000000000000000000, -0.000000000000000000, 0.000000000000000000 ) ) ;
#8498 = AXIS2_PLACEMENT_3D ( 'NONE', #2171, #8275, #9894 ) ;
#8499 = ORIENTED_EDGE ( 'NONE', *, *, #16475, .F. ) ;
#8500 = CARTESIAN_POINT ( 'NONE',  ( 8.812499995903225525, 5.763142191869157216, -0.3020334839682480288 ) ) ;
#8501 = FACE_OUTER_BOUND ( 'NONE', #7912, .T. ) ;
#8502 = CARTESIAN_POINT ( 'NONE',  ( 4.781284448697187273, -1.016293382781444654, -10.84374999795161543 ) ) ;
#8503 = CARTESIAN_POINT ( 'NONE',  ( 9.968749997951617203, -4.150607464521772094, -2.695436003842760275 ) ) ;
#8504 = CARTESIAN_POINT ( 'NONE',  ( 5.700000000000001066, 0.000000000000000000, -13.97977757194595760 ) ) ;
#8505 = CARTESIAN_POINT ( 'NONE',  ( -3.499494075959816541, 3.499494075959816541, -9.343749997951615427 ) ) ;
#8506 = EDGE_LOOP ( 'NONE', ( #11164, #5333, #2890, #764 ) ) ;
#8507 = CARTESIAN_POINT ( 'NONE',  ( 12.50000000000000533, 4.840010801796527318, -3.143139765844555900 ) ) ;
#8508 = EDGE_CURVE ( 'NONE', #2009, #5745, #11696, .T. ) ;
#8509 = CARTESIAN_POINT ( 'NONE',  ( 5.700000000000002842, 2.725425358843983450E-16, -10.64522241986047568 ) ) ;
#8510 = AXIS2_PLACEMENT_3D ( 'NONE', #16839, #14222, #11122 ) ;
#8511 = ORIENTED_EDGE ( 'NONE', *, *, #6063, .F. ) ;
#8512 = PRESENTATION_STYLE_ASSIGNMENT (( #4001 ) ) ;
#8513 = CIRCLE ( 'NONE', #16187, 7.500000000000000000 ) ;
#8514 = CARTESIAN_POINT ( 'NONE',  ( -14.19790265903626647, 9.644882309621941374, -32.00000000000000000 ) ) ;
#8515 = CARTESIAN_POINT ( 'NONE',  ( 4.476417968967386862, 17.43449690031536292, 32.00000000000000000 ) ) ;
#8516 = DIRECTION ( 'NONE',  ( 1.000000000000000000, 0.000000000000000000, 0.000000000000000000 ) ) ;
#8517 = VERTEX_POINT ( 'NONE', #8796 ) ;
#8518 = CARTESIAN_POINT ( 'NONE',  ( 111.3234999999999957, 0.000000000000000000, 0.000000000000000000 ) ) ;
#8519 = CARTESIAN_POINT ( 'NONE',  ( 4.200000000000001066, 0.000000000000000000, 0.000000000000000000 ) ) ;
#8520 = EDGE_LOOP ( 'NONE', ( #3112, #4541, #3044, #14985 ) ) ;
#8521 = CARTESIAN_POINT ( 'NONE',  ( -0.2436698586202288019, 0.000000000000000000, 7.174999999999998934 ) ) ;
#8522 = CIRCLE ( 'NONE', #19694, 6.735000000000022524 ) ;
#8523 = ORIENTED_EDGE ( 'NONE', *, *, #9282, .T. ) ;
#8524 = DIRECTION ( 'NONE',  ( -0.000000000000000000, 0.000000000000000000, 1.000000000000000000 ) ) ;
#8525 = CIRCLE ( 'NONE', #18428, 12.00000000000000178 ) ;
#8526 = DIRECTION ( 'NONE',  ( 0.000000000000000000, 0.000000000000000000, 1.000000000000000000 ) ) ;
#8527 = CARTESIAN_POINT ( 'NONE',  ( 13.00000000000000000, 0.2080849974989116558, 4.883670121236158401 ) ) ;
#8528 = CARTESIAN_POINT ( 'NONE',  ( -8.671566133830875600, 15.77352024078954429, -32.00000000000000000 ) ) ;
#8529 = VERTEX_POINT ( 'NONE', #10205 ) ;
#8530 = FACE_BOUND ( 'NONE', #10911, .T. ) ;
#8531 = CARTESIAN_POINT ( 'NONE',  ( 0.5109457054261454800, -4.861323657744410554, -14.46874999795161720 ) ) ;
#8532 = VERTEX_POINT ( 'NONE', #16302 ) ;
#8533 = AXIS2_PLACEMENT_3D ( 'NONE', #3169, #9279, #4675 ) ;
#8534 = EDGE_CURVE ( 'NONE', #12283, #8429, #16257, .T. ) ;
#8535 = CIRCLE ( 'NONE', #10773, 1.000000000000000888 ) ;
#8536 = FACE_OUTER_BOUND ( 'NONE', #10028, .T. ) ;
#8537 = CARTESIAN_POINT ( 'NONE',  ( 4.080749450109621534, -4.080749450109678378, -9.812499995903223748 ) ) ;
#8538 = ORIENTED_EDGE ( 'NONE', *, *, #1149, .T. ) ;
#8539 = B_SPLINE_CURVE_WITH_KNOTS ( 'NONE', 3,
 ( #9809, #2381, #14791, #15901 ),
 .UNSPECIFIED., .F., .F.,
 ( 4, 4 ),
 ( 2.135345996173297489E-07, 0.0006888010880210770339 ),
 .UNSPECIFIED. ) ;
#8540 = CARTESIAN_POINT ( 'NONE',  ( 0.000000000000000000, 0.000000000000000000, -28.99999999999999645 ) ) ;
#8541 = CARTESIAN_POINT ( 'NONE',  ( -4.080749450109677490, -4.080749450109622423, -13.50000000000000533 ) ) ;
#8542 = FACE_BOUND ( 'NONE', #1966, .T. ) ;
#8543 = ORIENTED_EDGE ( 'NONE', *, *, #12633, .F. ) ;
#8544 = DIRECTION ( 'NONE',  ( 1.000000000000000000, 0.000000000000000000, 0.000000000000000000 ) ) ;
#8545 = ORIENTED_EDGE ( 'NONE', *, *, #17565, .T. ) ;
#8546 = CARTESIAN_POINT ( 'NONE',  ( 13.00000000000000178, -4.568735188514048140, -1.737869959597788672 ) ) ;
#8547 = CARTESIAN_POINT ( 'NONE',  ( 1.749999999999998002, -25.12109765559643648, -12.52377138324252570 ) ) ;
#8548 = DIRECTION ( 'NONE',  ( -1.000000000000000000, -0.000000000000000000, -0.000000000000000000 ) ) ;
#8549 = ORIENTED_EDGE ( 'NONE', *, *, #19313, .T. ) ;
#8550 = DIRECTION ( 'NONE',  ( 0.000000000000000000, 0.000000000000000000, -1.000000000000000000 ) ) ;
#8551 = CARTESIAN_POINT ( 'NONE',  ( 10.31249999590322552, -4.611396867937225252, 3.350375938067065462 ) ) ;
#8552 = CIRCLE ( 'NONE', #17174, 0.2000000000000005107 ) ;
#8553 = FACE_OUTER_BOUND ( 'NONE', #12626, .T. ) ;
#8554 = AXIS2_PLACEMENT_3D ( 'NONE', #5249, #12964, #3653 ) ;
#8555 = ORIENTED_EDGE ( 'NONE', *, *, #19538, .T. ) ;
#8556 = ADVANCED_FACE ( 'NONE', ( #16501 ), #13203, .F. ) ;
#8557 = ORIENTED_EDGE ( 'NONE', *, *, #14677, .T. ) ;
#8558 = EDGE_CURVE ( 'NONE', #13272, #4315, #10501, .T. ) ;
#8559 = CARTESIAN_POINT ( 'NONE',  ( 2.601776105308174269, 25.78859396478527799, 2.857713464478781162 ) ) ;
#8560 = AXIS2_PLACEMENT_3D ( 'NONE', #8528, #10332, #14636 ) ;
#8561 = DIRECTION ( 'NONE',  ( -1.000000000000000000, 0.000000000000000000, 0.000000000000000000 ) ) ;
#8562 = ORIENTED_EDGE ( 'NONE', *, *, #6751, .F. ) ;
#8563 = CARTESIAN_POINT ( 'NONE',  ( 6.468749997951615427, -4.233219804643904460, 2.444050593749960587 ) ) ;
#8564 = CARTESIAN_POINT ( 'NONE',  ( -2.444050593750049849, -4.233219804643852946, -6.843749997951615427 ) ) ;
#8565 = ORIENTED_EDGE ( 'NONE', *, *, #13701, .T. ) ;
#8566 = ORIENTED_EDGE ( 'NONE', *, *, #16277, .F. ) ;
#8567 = CARTESIAN_POINT ( 'NONE',  ( 0.000000000000000000, 4.898587196589412829E-16, -4.000000000000000000 ) ) ;
#8568 = DIRECTION ( 'NONE',  ( -1.000000000000000000, 0.000000000000000000, 0.000000000000000000 ) ) ;
#8569 = EDGE_CURVE ( 'NONE', #10979, #19457, #16600, .T. ) ;
#8570 = AXIS2_PLACEMENT_3D ( 'NONE', #158, #17068, #12462 ) ;
#8571 = LINE ( 'NONE', #6759, #13600 ) ;
#8572 = ORIENTED_EDGE ( 'NONE', *, *, #1660, .T. ) ;
#8573 = LINE ( 'NONE', #19467, #2611 ) ;
#8574 = CARTESIAN_POINT ( 'NONE',  ( 12.34374999795161543, 3.114526743279308896, -3.846120219227901149 ) ) ;
#8575 = ADVANCED_FACE ( 'NONE', ( #19488 ), #2580, .T. ) ;
#8576 = VERTEX_POINT ( 'NONE', #4292 ) ;
#8577 = DIRECTION ( 'NONE',  ( 1.000000000000000000, 0.000000000000000000, 0.000000000000000000 ) ) ;
#8578 = ADVANCED_FACE ( 'NONE', ( #8896 ), #13294, .F. ) ;
#8579 = DIRECTION ( 'NONE',  ( 0.000000000000000000, 0.000000000000000000, 1.000000000000000000 ) ) ;
#8580 = CARTESIAN_POINT ( 'NONE',  ( 0.001865824574860882289, 20.90825775245787455, -12.51925356660738053 ) ) ;
#8581 = CARTESIAN_POINT ( 'NONE',  ( 2.718184743034447237, -24.78695292654925808, 5.344212458769271201 ) ) ;
#8582 = CIRCLE ( 'NONE', #16587, 22.00000000000000355 ) ;
#8583 = CARTESIAN_POINT ( 'NONE',  ( 2.500000000000002220, 8.130889342088982951E-16, -6.543750000000017941 ) ) ;
#8584 =( NAMED_UNIT ( * ) PLANE_ANGLE_UNIT ( ) SI_UNIT ( $, .RADIAN. ) );
#8585 = CARTESIAN_POINT ( 'NONE',  ( 2.789999999999999147, -12.52067188844336165, -20.62201879784926462 ) ) ;
#8586 = EDGE_LOOP ( 'NONE', ( #10724, #14001, #10235, #2849, #7896, #2931 ) ) ;
#8587 = ADVANCED_FACE ( 'NONE', ( #18201 ), #11997, .T. ) ;
#8588 = ADVANCED_FACE ( 'NONE', ( #1585 ), #1018, .T. ) ;
#8589 = DIRECTION ( 'NONE',  ( 1.000000000000000000, 0.000000000000000000, 0.000000000000000000 ) ) ;
#8590 = DIRECTION ( 'NONE',  ( 0.000000000000000000, 0.000000000000000000, 1.000000000000000000 ) ) ;
#8591 = UNCERTAINTY_MEASURE_WITH_UNIT (LENGTH_MEASURE( 1.000000000000000082E-05 ), #14093, 'distance_accuracy_value', 'NONE');
#8592 = CARTESIAN_POINT ( 'NONE',  ( 1.280903732194421663, -4.780397808154265960, -14.34374999795161365 ) ) ;
#8593 = STYLED_ITEM ( 'NONE', ( #17766 ), #14973 ) ;
#8594 = CARTESIAN_POINT ( 'NONE',  ( -90.00000000000000000, 0.000000000000000000, 0.000000000000000000 ) ) ;
#8595 = CARTESIAN_POINT ( 'NONE',  ( -4.648860486681953397, 1.510506337161861445, -7.843749997951614539 ) ) ;
#8596 = EDGE_CURVE ( 'NONE', #18489, #9581, #4848, .T. ) ;
#8597 = VERTEX_POINT ( 'NONE', #15592 ) ;
#8598 = DIRECTION ( 'NONE',  ( -0.000000000000000000, -0.000000000000000000, 1.000000000000000000 ) ) ;
#8599 = DIRECTION ( 'NONE',  ( 0.000000000000000000, -0.000000000000000000, -1.000000000000000000 ) ) ;
#8600 = AXIS2_PLACEMENT_3D ( 'NONE', #2057, #15872, #11171 ) ;
#8601 = ORIENTED_EDGE ( 'NONE', *, *, #3552, .T. ) ;
#8602 = CARTESIAN_POINT ( 'NONE',  ( -14.19790265903626647, 9.644882309621941374, 32.00000000000000000 ) ) ;
#8603 = DIRECTION ( 'NONE',  ( 0.000000000000000000, 0.000000000000000000, -1.000000000000000000 ) ) ;
#8604 = FACE_OUTER_BOUND ( 'NONE', #19261, .T. ) ;
#8605 = CARTESIAN_POINT ( 'NONE',  ( -5.209999999999999964, 0.000000000000000000, 0.000000000000000000 ) ) ;
#8606 = DIRECTION ( 'NONE',  ( 1.000000000000000000, 1.776356839400250465E-15, 0.000000000000000000 ) ) ;
#8607 = EDGE_LOOP ( 'NONE', ( #1289, #17108 ) ) ;
#8608 = CARTESIAN_POINT ( 'NONE',  ( -6.626241948324210540, -16.73597674598852336, 35.00000000000000000 ) ) ;
#8609 = CARTESIAN_POINT ( 'NONE',  ( 2.444050593750020095, 4.233219804643871598, -6.843749997951615427 ) ) ;
#8610 = ADVANCED_FACE ( 'NONE', ( #19465 ), #12489, .F. ) ;
#8611 = CARTESIAN_POINT ( 'NONE',  ( 0.000000000000000000, 2.680914349914567470E-13, -25.59481291497571220 ) ) ;
#8612 = EDGE_LOOP ( 'NONE', ( #916, #19524 ) ) ;
#8613 = CARTESIAN_POINT ( 'NONE',  ( 10.58013454126452046, -14.56230589874905412, 32.00000000000000000 ) ) ;
#8614 = ORIENTED_EDGE ( 'NONE', *, *, #2854, .T. ) ;
#8615 = CARTESIAN_POINT ( 'NONE',  ( 0.02436607992776455150, 21.30679549418631780, 12.59161484032919986 ) ) ;
#8616 = CARTESIAN_POINT ( 'NONE',  ( -5.142044285764751699, 2.620002426024544029, -8.812499995903225525 ) ) ;
#8617 = FACE_OUTER_BOUND ( 'NONE', #16078, .T. ) ;
#8618 = VECTOR ( 'NONE', #16641, 1000.000000000000000 ) ;
#8619 = CARTESIAN_POINT ( 'NONE',  ( 11.58013454126452579, -14.56230589874905412, -35.00000000000000000 ) ) ;
#8620 = ORIENTED_EDGE ( 'NONE', *, *, #12769, .F. ) ;
#8621 = CARTESIAN_POINT ( 'NONE',  ( 2.257825462012206685, 12.96514671151767395, 23.74442027961364943 ) ) ;
#8622 = LINE ( 'NONE', #4120, #847 ) ;
#8623 = VERTEX_POINT ( 'NONE', #10890 ) ;
#8624 = CYLINDRICAL_SURFACE ( 'NONE', #13466, 5.400000000000000355 ) ;
#8625 = CARTESIAN_POINT ( 'NONE',  ( -2.246813503491864150, -4.409619785863891472, -13.34374999795161365 ) ) ;
#8626 = B_SPLINE_CURVE_WITH_KNOTS ( 'NONE', 3,
 ( #16430, #7196, #8920, #15023, #9018, #2704 ),
 .UNSPECIFIED., .F., .F.,
 ( 4, 2, 4 ),
 ( 2.321268216997094965E-07, 0.001878622960950493588, 0.003757013795079287150 ),
 .UNSPECIFIED. ) ;
#8627 = ORIENTED_EDGE ( 'NONE', *, *, #892, .T. ) ;
#8629 = DIRECTION ( 'NONE',  ( 1.000000000000000000, 0.000000000000000000, 0.000000000000000000 ) ) ;
#8628 = VECTOR ( 'NONE', #12389, 1000.000000000000000 ) ;
#8630 = B_SPLINE_CURVE_WITH_KNOTS ( 'NONE', 1,
 ( #15550, #15748 ),
 .UNSPECIFIED., .F., .F.,
 ( 2, 2 ),
 ( 0.000000000000000000, 1.000000000000000000 ),
 .UNSPECIFIED. ) ;
#8631 = CARTESIAN_POINT ( 'NONE',  ( 0.9027913098498173694, -5.700000000000006395, -10.50000000000000533 ) ) ;
#8632 = AXIS2_PLACEMENT_3D ( 'NONE', #225, #18720, #10830 ) ;
#8633 = FACE_BOUND ( 'NONE', #2917, .T. ) ;
#8634 = EDGE_CURVE ( 'NONE', #4629, #5305, #5480, .T. ) ;
#8635 = ORIENTED_EDGE ( 'NONE', *, *, #10886, .F. ) ;
#8636 = DIRECTION ( 'NONE',  ( 0.000000000000000000, 0.000000000000000000, 1.000000000000000000 ) ) ;
#8637 = ORIENTED_EDGE ( 'NONE', *, *, #6299, .F. ) ;
#8638 = DIRECTION ( 'NONE',  ( 1.000000000000000000, 0.000000000000000000, 0.000000000000000000 ) ) ;
#8639 = ORIENTED_EDGE ( 'NONE', *, *, #5348, .F. ) ;
#8640 = DIRECTION ( 'NONE',  ( 0.000000000000000000, 0.9510565162951567508, -0.3090169943749379589 ) ) ;
#8641 = DIRECTION ( 'NONE',  ( 0.9945218953682738450, 0.1045284632676491549, 0.000000000000000000 ) ) ;
#8642 = CARTESIAN_POINT ( 'NONE',  ( 16.96448111170888851, 1.130229351527639370, 32.00000000000000000 ) ) ;
#8643 = VERTEX_POINT ( 'NONE', #376 ) ;
#8644 = CARTESIAN_POINT ( 'NONE',  ( -0.7741991708319226895, -4.888101187499994893, -11.96874999795161365 ) ) ;
#8645 = CARTESIAN_POINT ( 'NONE',  ( 1.039999999999997149, -24.89775460606822577, -12.96210679857813730 ) ) ;
#8646 = DIRECTION ( 'NONE',  ( -0.000000000000000000, -0.000000000000000000, 1.000000000000000000 ) ) ;
#8647 = EDGE_CURVE ( 'NONE', #10762, #10821, #18414, .T. ) ;
#8648 = VERTEX_POINT ( 'NONE', #10987 ) ;
#8649 = VECTOR ( 'NONE', #7775, 1000.000000000000000 ) ;
#8650 = DIRECTION ( 'NONE',  ( 0.000000000000000000, 0.000000000000000000, 1.000000000000000000 ) ) ;
#8651 = ORIENTED_EDGE ( 'NONE', *, *, #10749, .T. ) ;
#8652 = EDGE_CURVE ( 'NONE', #9276, #12478, #16701, .T. ) ;
#8653 = CARTESIAN_POINT ( 'NONE',  ( -41.99999999999999289, -5.000000000000001776, 2.000000000000000000 ) ) ;
#8654 = DIRECTION ( 'NONE',  ( 0.000000000000000000, -1.000000000000000000, 0.000000000000000000 ) ) ;
#8655 = EDGE_LOOP ( 'NONE', ( #10174, #13317, #747, #14702 ) ) ;
#8656 = CARTESIAN_POINT ( 'NONE',  ( 2.789999999999999147, -25.59481291497571220, -1.787276233276378314E-13 ) ) ;
#8657 = AXIS2_PLACEMENT_3D ( 'NONE', #1296, #18013, #1496 ) ;
#8658 = SHAPE_REPRESENTATION_RELATIONSHIP ( 'NONE' , 'NONE' ,  #19604, #14973 ) ;
#8659 = FACE_OUTER_BOUND ( 'NONE', #10430, .T. ) ;
#8660 = VERTEX_POINT ( 'NONE', #16996 ) ;
#8661 = ORIENTED_EDGE ( 'NONE', *, *, #1414, .T. ) ;
#8662 = DIRECTION ( 'NONE',  ( 0.000000000000000000, 0.000000000000000000, 1.000000000000000000 ) ) ;
#8663 = FACE_OUTER_BOUND ( 'NONE', #13153, .T. ) ;
#8664 = EDGE_CURVE ( 'NONE', #3813, #14128, #7066, .T. ) ;
#8665 = ORIENTED_EDGE ( 'NONE', *, *, #6055, .T. ) ;
#8666 = DIRECTION ( 'NONE',  ( -1.000000000000000000, -0.000000000000000000, -0.000000000000000000 ) ) ;
#8667 = ORIENTED_EDGE ( 'NONE', *, *, #7334, .T. ) ;
#8668 = DIRECTION ( 'NONE',  ( 0.000000000000000000, 0.000000000000000000, 1.000000000000000000 ) ) ;
#8669 = CARTESIAN_POINT ( 'NONE',  ( 13.00000000000000888, -4.521642095224331470, -1.858077407906666867 ) ) ;
#8670 = AXIS2_PLACEMENT_3D ( 'NONE', #5126, #2034, #17054 ) ;
#8671 = ORIENTED_EDGE ( 'NONE', *, *, #5422, .F. ) ;
#8672 = DIRECTION ( 'NONE',  ( 0.000000000000000000, 0.000000000000000000, -1.000000000000000000 ) ) ;
#8673 = VECTOR ( 'NONE', #19292, 1000.000000000000000 ) ;
#8674 = AXIS2_PLACEMENT_3D ( 'NONE', #2530, #16250, #17558 ) ;
#8675 = B_SPLINE_CURVE_WITH_KNOTS ( 'NONE', 3,
 ( #19690, #5973, #7574, #4190, #16597, #16804, #1190, #10402, #4290, #13691 ),
 .UNSPECIFIED., .F., .F.,
 ( 4, 3, 3, 4 ),
 ( 0.000000000000000000, 0.0001875345074742622623, 0.0003808595644229699441, 0.0005744879655065562602 ),
 .UNSPECIFIED. ) ;
#8676 = CARTESIAN_POINT ( 'NONE',  ( -5.626241948324210540, -16.73597674598852336, -35.00000000000000000 ) ) ;
#8677 = CARTESIAN_POINT ( 'NONE',  ( 0.000000000000000000, -5.000000000000001776, 41.99999999999999289 ) ) ;
#8678 = EDGE_CURVE ( 'NONE', #2569, #9700, #18278, .T. ) ;
#8679 = CARTESIAN_POINT ( 'NONE',  ( 2.789999999999999147, 14.55412442567645215, -19.64056340710859772 ) ) ;
#8680 = CARTESIAN_POINT ( 'NONE',  ( -7.671566133830872047, 15.77352024078954429, 35.00000000000000000 ) ) ;
#8681 = FILL_AREA_STYLE ('',( #11786 ) ) ;
#8682 = CARTESIAN_POINT ( 'NONE',  ( 0.02436607992775761261, 22.71065055754452544, 9.836394144775786330 ) ) ;
#8683 = ORIENTED_EDGE ( 'NONE', *, *, #16066, .T. ) ;
#8684 = CARTESIAN_POINT ( 'NONE',  ( 2.790000000000000924, 0.000000000000000000, 0.000000000000000000 ) ) ;
#8685 = EDGE_CURVE ( 'NONE', #7717, #11676, #3571, .T. ) ;
#8686 = AXIS2_PLACEMENT_3D ( 'NONE', #1319, #8924, #4419 ) ;
#8687 = CARTESIAN_POINT ( 'NONE',  ( 2.765633920072239516, -24.63872515616084513, 2.336989772644183283 ) ) ;
#8688 = AXIS2_PLACEMENT_3D ( 'NONE', #14214, #18809, #517 ) ;
#8689 = DIRECTION ( 'NONE',  ( 1.000000000000000000, 0.000000000000000000, 0.000000000000000000 ) ) ;
#8690 = EDGE_CURVE ( 'NONE', #5418, #12054, #6123, .T. ) ;
#8691 = CARTESIAN_POINT ( 'NONE',  ( 4.781284448697187273, -1.016293382781444654, -10.46874999795161720 ) ) ;
#8692 = CARTESIAN_POINT ( 'NONE',  ( 1.749999999999998002, -12.52377138324241734, 25.12109765559649688 ) ) ;
#8693 = EDGE_LOOP ( 'NONE', ( #7090, #10374, #3699, #7423 ) ) ;
#8694 = CARTESIAN_POINT ( 'NONE',  ( 2.789999999999999147, 7.772527002114753003, -23.17675759782032685 ) ) ;
#8695 = VECTOR ( 'NONE', #982, 1000.000000000000000 ) ;
#8696 = CARTESIAN_POINT ( 'NONE',  ( 2.765633920072237295, 12.59161484032912171, 21.30679549418635688 ) ) ;
#8697 = ORIENTED_EDGE ( 'NONE', *, *, #9093, .F. ) ;
#8698 = CARTESIAN_POINT ( 'NONE',  ( 11.31249999590322375, -1.185096637661254171, 5.575441324182689229 ) ) ;
#8699 = DIRECTION ( 'NONE',  ( 1.000000000000000000, 0.000000000000000000, 0.000000000000000000 ) ) ;
#8700 = AXIS2_PLACEMENT_3D ( 'NONE', #12993, #8579, #11393 ) ;
#8701 = CARTESIAN_POINT ( 'NONE',  ( -5.209999999999999964, 0.000000000000000000, 0.000000000000000000 ) ) ;
#8702 = PRODUCT_RELATED_PRODUCT_CATEGORY ( 'part', '', ( #4114 ) ) ;
#8703 = ORIENTED_EDGE ( 'NONE', *, *, #13139, .F. ) ;
#8704 = B_SPLINE_CURVE_WITH_KNOTS ( 'NONE', 1,
 ( #17913, #2893 ),
 .UNSPECIFIED., .F., .F.,
 ( 2, 2 ),
 ( 0.000000000000000000, 1.000000000000000000 ),
 .UNSPECIFIED. ) ;
#8705 = FACE_OUTER_BOUND ( 'NONE', #3173, .T. ) ;
#8706 = DIRECTION ( 'NONE',  ( 0.000000000000000000, 0.000000000000000000, 1.000000000000000000 ) ) ;
#8707 = TOROIDAL_SURFACE ( 'NONE', #741, 24.12539914357697413, 8.000000000000000000 ) ;
#8708 = DIRECTION ( 'NONE',  ( -1.000000000000000000, 0.000000000000000000, 0.000000000000000000 ) ) ;
#8709 = EDGE_LOOP ( 'NONE', ( #10336, #16094 ) ) ;
#8710 = FACE_OUTER_BOUND ( 'NONE', #4627, .T. ) ;
#8711 = VERTEX_POINT ( 'NONE', #13693 ) ;
#8712 = ADVANCED_FACE ( 'NONE', ( #9097, #12590 ), #6075, .F. ) ;
#8713 = CARTESIAN_POINT ( 'NONE',  ( 0.1855657389739094887, -5.253342437939553022, -25.39738473785006079 ) ) ;
#8714 = EDGE_CURVE ( 'NONE', #6321, #4362, #3384, .T. ) ;
#8715 = CARTESIAN_POINT ( 'NONE',  ( 2.262072625383131363, 26.57710921259761960, 4.996265754456460151 ) ) ;
#8716 = VECTOR ( 'NONE', #18766, 1000.000000000000000 ) ;
#8717 = CARTESIAN_POINT ( 'NONE',  ( 1.761396867937200073, 5.421022142882376826, -12.00000000000000533 ) ) ;
#8718 = VERTEX_POINT ( 'NONE', #3080 ) ;
#8719 = CARTESIAN_POINT ( 'NONE',  ( -1.988169868018624609, -4.465502636338009701, -9.468749997951615427 ) ) ;
#8720 = CARTESIAN_POINT ( 'NONE',  ( 5.510910596163084625E-16, 18.00000000000000355, 35.00000000000000000 ) ) ;
#8721 = ORIENTED_EDGE ( 'NONE', *, *, #2684, .T. ) ;
#8722 = CLOSED_SHELL ( 'NONE', ( #18105, #2545, #17318, #6876, #10307, #4780, #10227, #12644, #15569, #7424, #2802, #5702, #11346, #19619, #18550, #10898, #1637, #10274, #11412, #1461, #18607, #13331, #638, #746, #1993, #6499, #19281, #13349, #6383, #244, #13426, #11299, #7397, #11165, #15868, #8908, #1739, #3761, #6130, #3315, #5849, #19122, #17776, #5693, #15820, #13971, #14827, #811, #12281, #15401, #16509, #7350, #10373, #17113, #18947, #17507, #9776, #19134, #18535, #4062, #2556, #10282, #7074, #19352, #17280, #4433, #16283, #11130, #10412, #12400, #17277, #19184, #9008, #12885, #16256, #1094, #18261, #6905, #7444, #1191, #3361, #938, #18252, #11716, #3023, #2069, #17292, #5685, #14547, #8334, #17002, #1078, #8575, #7850, #8282, #6553, #6494, #15275, #15336, #7951, #18870, #1625, #8610, #950, #3372, #14570, #5376, #7453, #15081, #2513, #8105, #13991, #26, #8414, #1376, #16138, #11127, #15297, #16163, #15213, #15485, #8150, #10131, #6587, #12596, #4871, #7240, #2443, #2351, #2601, #1801, #966, #9248 ) ) ;
#8723 = EDGE_CURVE ( 'NONE', #11430, #9260, #4484, .T. ) ;
#8724 = AXIS2_PLACEMENT_3D ( 'NONE', #19239, #11455, #5532 ) ;
#8725 = CARTESIAN_POINT ( 'NONE',  ( 4.476417968967386862, 17.43449690031536292, 32.00000000000000000 ) ) ;
#8726 = DIRECTION ( 'NONE',  ( -1.000000000000000000, -0.000000000000000000, -0.000000000000000000 ) ) ;
#8727 = ADVANCED_FACE ( 'NONE', ( #4686 ), #5635, .F. ) ;
#8728 = ORIENTED_EDGE ( 'NONE', *, *, #1048, .F. ) ;
#8729 = STYLED_ITEM ( 'NONE', ( #822 ), #10191 ) ;
#8730 = CARTESIAN_POINT ( 'NONE',  ( 4.861323657744406113, -0.5109457054261780096, -13.46874999795161543 ) ) ;
#8731 = DIRECTION ( 'NONE',  ( -1.000000000000000000, 0.000000000000000000, 0.000000000000000000 ) ) ;
#8732 = EDGE_CURVE ( 'NONE', #17039, #14026, #784, .T. ) ;
#8733 = LINE ( 'NONE', #7206, #8752 ) ;
#8734 = ORIENTED_EDGE ( 'NONE', *, *, #19165, .T. ) ;
#8735 = CARTESIAN_POINT ( 'NONE',  ( 91.50000000000000000, 0.000000000000000000, -4.000000000000000000 ) ) ;
#8736 = ORIENTED_EDGE ( 'NONE', *, *, #18220, .T. ) ;
#8737 = CARTESIAN_POINT ( 'NONE',  ( 2.789999999999999147, -0.2301004812055740811, -24.44424927289185590 ) ) ;
#8738 = ORIENTED_EDGE ( 'NONE', *, *, #12144, .F. ) ;
#8739 = CARTESIAN_POINT ( 'NONE',  ( -2.000000000000001776, 7.960204194457801393E-16, -6.500000000000000888 ) ) ;
#8740 = CARTESIAN_POINT ( 'NONE',  ( -3.476417968967383754, 17.43449690031536292, 32.00000000000000000 ) ) ;
#8741 = CARTESIAN_POINT ( 'NONE',  ( 0.7741991708318548548, -4.888101187500005551, -11.34374999795161543 ) ) ;
#8742 = DIRECTION ( 'NONE',  ( 0.000000000000000000, 0.000000000000000000, -1.000000000000000000 ) ) ;
#8743 = DIRECTION ( 'NONE',  ( 0.000000000000000000, 0.7315216790650488354, 0.6818181818181822118 ) ) ;
#8744 = ORIENTED_EDGE ( 'NONE', *, *, #4850, .F. ) ;
#8745 = MECHANICAL_DESIGN_GEOMETRIC_PRESENTATION_REPRESENTATION (  '', ( #4264 ), #6806 ) ;
#8746 = B_SPLINE_CURVE_WITH_KNOTS ( 'NONE', 3,
 ( #12953, #849, #3020, #16445, #14937, #2913 ),
 .UNSPECIFIED., .F., .F.,
 ( 4, 2, 4 ),
 ( 4.462636678184503380E-07, 0.001879885020955184395, 0.003759323778242550443 ),
 .UNSPECIFIED. ) ;
#8747 = DIRECTION ( 'NONE',  ( 0.000000000000000000, 0.000000000000000000, 1.000000000000000000 ) ) ;
#8748 = EDGE_CURVE ( 'NONE', #3405, #10636, #5166, .T. ) ;
#8749 = PRODUCT_DEFINITION_SHAPE ( 'NONE', 'NONE',  #19793 ) ;
#8750 = EDGE_LOOP ( 'NONE', ( #13870, #740, #15832, #16935, #19267, #7736 ) ) ;
#8751 = CLOSED_SHELL ( 'NONE', ( #14882, #17525, #6057, #16932, #5269, #4266, #15195, #19573, #3120, #11263, #1589, #4146, #4320, #13846, #2515, #15239, #15629, #10796, #1719, #16635 ) ) ;
#8752 = VECTOR ( 'NONE', #13329, 1000.000000000000000 ) ;
#8753 = LINE ( 'NONE', #8855, #16330 ) ;
#8754 = EDGE_CURVE ( 'NONE', #13082, #17341, #16358, .T. ) ;
#8755 = CARTESIAN_POINT ( 'NONE',  ( -5.294050593750000644, 0.000000000000000000, -7.078124996927420476 ) ) ;
#8756 = DIRECTION ( 'NONE',  ( 0.000000000000000000, 0.000000000000000000, 1.000000000000000000 ) ) ;
#8757 = EDGE_CURVE ( 'NONE', #16011, #15888, #7724, .T. ) ;
#8758 = DIRECTION ( 'NONE',  ( -1.000000000000000000, -0.000000000000000000, -0.000000000000000000 ) ) ;
#8759 = ORIENTED_EDGE ( 'NONE', *, *, #84, .T. ) ;
#8760 = CARTESIAN_POINT ( 'NONE',  ( -0.5109457054261112852, 4.861323657744413218, -14.84374999795161543 ) ) ;
#8761 = STYLED_ITEM ( 'NONE', ( #17081 ), #7075 ) ;
#8762 = CIRCLE ( 'NONE', #19302, 1.000000000000002442 ) ;
#8763 = DIRECTION ( 'NONE',  ( 0.000000000000000000, 6.419766481290788001E-33, -1.000000000000000000 ) ) ;
#8764 = CARTESIAN_POINT ( 'NONE',  ( 4.780397808154257078, -1.280903732194453859, -13.96874999795161365 ) ) ;
#8765 = DIRECTION ( 'NONE',  ( 0.000000000000000000, 0.000000000000000000, 1.000000000000000000 ) ) ;
#8766 = VERTEX_POINT ( 'NONE', #683 ) ;
#8767 = VERTEX_POINT ( 'NONE', #12786 ) ;
#8768 = DIRECTION ( 'NONE',  ( -1.000000000000000000, 0.000000000000000000, 0.000000000000000000 ) ) ;
#8769 = EDGE_CURVE ( 'NONE', #16782, #2569, #5169, .T. ) ;
#8770 = CARTESIAN_POINT ( 'NONE',  ( 6.000000000000005329, 4.936344801571289409, 2.850000000000024070 ) ) ;
#8771 = ORIENTED_EDGE ( 'NONE', *, *, #8829, .T. ) ;
#8772 = CARTESIAN_POINT ( 'NONE',  ( 3.143139765844623401, 4.840010801796481132, -9.500000000000005329 ) ) ;
#8773 = VERTEX_POINT ( 'NONE', #17583 ) ;
#8774 = CARTESIAN_POINT ( 'NONE',  ( -8.671566133830875600, 15.77352024078954429, 32.00000000000000000 ) ) ;
#8775 = CARTESIAN_POINT ( 'NONE',  ( 0.02436607992776194942, -5.391175441198450713, -24.15498966839968276 ) ) ;
#8776 = COLOUR_RGB ( '', 0.31764706, 0.68627451, 0.89019608) ;
#8777 = ORIENTED_EDGE ( 'NONE', *, *, #7039, .T. ) ;
#8778 = DIRECTION ( 'NONE',  ( 0.000000000000000000, 1.000000000000000000, 0.000000000000000000 ) ) ;
#8779 = EDGE_CURVE ( 'NONE', #14268, #3988, #10298, .T. ) ;
#8780 = CIRCLE ( 'NONE', #160, 0.9999999999999974465 ) ;
#8781 = CARTESIAN_POINT ( 'NONE',  ( 2.783025228907523019, 9.686319561461266048, -22.53337530003393141 ) ) ;
#8782 = CARTESIAN_POINT ( 'NONE',  ( 15.31249999590322552, 3.350375938067097881, 4.611396867937200383 ) ) ;
#8783 = DIRECTION ( 'NONE',  ( 1.000000000000000000, 0.000000000000000000, 0.000000000000000000 ) ) ;
#8784 = DIRECTION ( 'NONE',  ( -1.000000000000000000, -0.000000000000000000, -0.000000000000000000 ) ) ;
#8785 =( NAMED_UNIT ( * ) PLANE_ANGLE_UNIT ( ) SI_UNIT ( $, .RADIAN. ) );
#8786 = CARTESIAN_POINT ( 'NONE',  ( -30.00000000000000000, -8.000000000000000000, 9.797174393178825657E-16 ) ) ;
#8787 = ORIENTED_EDGE ( 'NONE', *, *, #4784, .F. ) ;
#8788 = CARTESIAN_POINT ( 'NONE',  ( -4.888101187500000222, 0.000000000000000000, -6.656249997951614539 ) ) ;
#8789 = AXIS2_PLACEMENT_3D ( 'NONE', #5447, #1047, #6939 ) ;
#8790 = CARTESIAN_POINT ( 'NONE',  ( 0.000000000000000000, 6.000000000000000000, 0.000000000000000000 ) ) ;
#8791 = UNCERTAINTY_MEASURE_WITH_UNIT (LENGTH_MEASURE( 1.000000000000000082E-05 ), #17620, 'distance_accuracy_value', 'NONE');
#8792 = DIRECTION ( 'NONE',  ( 0.000000000000000000, -1.000000000000000000, 0.000000000000000000 ) ) ;
#8793 = DIRECTION ( 'NONE',  ( -1.000000000000000000, 0.000000000000000000, 0.000000000000000000 ) ) ;
#8794 = DIRECTION ( 'NONE',  ( -1.000000000000000000, -0.000000000000000000, -0.000000000000000000 ) ) ;
#8795 = ORIENTED_EDGE ( 'NONE', *, *, #2648, .T. ) ;
#8796 = CARTESIAN_POINT ( 'NONE',  ( -2.500000000000002220, 8.130889342088985910E-16, 6.543750000000023270 ) ) ;
#8797 = EDGE_CURVE ( 'NONE', #11866, #9454, #14389, .T. ) ;
#8798 = DIRECTION ( 'NONE',  ( 1.000000000000000000, 0.000000000000000000, 0.000000000000000000 ) ) ;
#8799 = VERTEX_POINT ( 'NONE', #4979 ) ;
#8800 = CARTESIAN_POINT ( 'NONE',  ( 10.46874999795161720, 1.016293382781477961, -4.781284448697179279 ) ) ;
#8801 = CARTESIAN_POINT ( 'NONE',  ( 1.899999999999999023, 8.279592079675421725E-16, 6.760799999999997034 ) ) ;
#8802 = AXIS2_PLACEMENT_3D ( 'NONE', #4172, #19274, #7152 ) ;
#8803 = EDGE_CURVE ( 'NONE', #7464, #14997, #2074, .T. ) ;
#8804 = CIRCLE ( 'NONE', #834, 1.000000000000004441 ) ;
#8805 = CARTESIAN_POINT ( 'NONE',  ( -7.937500000000000000, 1.560264056424245815, -0.06840592591720176530 ) ) ;
#8806 = LINE ( 'NONE', #2788, #13213 ) ;
#8807 = ORIENTED_EDGE ( 'NONE', *, *, #17366, .T. ) ;
#8808 = LINE ( 'NONE', #4203, #19374 ) ;
#8809 = DIRECTION ( 'NONE',  ( 0.000000000000000000, 0.000000000000000000, 1.000000000000000000 ) ) ;
#8810 = PRESENTATION_STYLE_ASSIGNMENT (( #2693 ) ) ;
#8811 = ORIENTED_EDGE ( 'NONE', *, *, #12380, .T. ) ;
#8812 = CARTESIAN_POINT ( 'NONE',  ( 2.789999999999999147, -12.52067188844365830, 20.62201879784908698 ) ) ;
#8813 = EDGE_LOOP ( 'NONE', ( #3946, #4267, #320, #12559 ) ) ;
#8814 = CARTESIAN_POINT ( 'NONE',  ( 13.00000000000000000, -4.333424887442987483, -2.261628166637620119 ) ) ;
#8815 = DIRECTION ( 'NONE',  ( 0.000000000000000000, 0.000000000000000000, -1.000000000000000000 ) ) ;
#8816 = DIRECTION ( 'NONE',  ( 0.000000000000000000, 0.000000000000000000, 1.000000000000000000 ) ) ;
#8817 = AXIS2_PLACEMENT_3D ( 'NONE', #17964, #2939, #14957 ) ;
#8818 = CARTESIAN_POINT ( 'NONE',  ( 4.611396867937200383, 3.350375938067097881, -15.31249999590322552 ) ) ;
#8819 = AXIS2_PLACEMENT_3D ( 'NONE', #9223, #1612, #4713 ) ;
#8820 = ORIENTED_EDGE ( 'NONE', *, *, #14554, .F. ) ;
#8821 = FACE_OUTER_BOUND ( 'NONE', #13264, .T. ) ;
#8822 = EDGE_CURVE ( 'NONE', #17152, #8438, #2303, .T. ) ;
#8823 = PRODUCT_DEFINITION ( 'UNKNOWN', '', #5071, #8197 ) ;
#8824 = CARTESIAN_POINT ( 'NONE',  ( 2.999999999999998224, 0.000000000000000000, 0.000000000000000000 ) ) ;
#8825 = ORIENTED_EDGE ( 'NONE', *, *, #15331, .T. ) ;
#8826 = EDGE_CURVE ( 'NONE', #17528, #17855, #18596, .T. ) ;
#8827 = FACE_OUTER_BOUND ( 'NONE', #13812, .T. ) ;
#8828 = CARTESIAN_POINT ( 'NONE',  ( 0.7741991708318548548, -4.888101187500005551, -11.34374999795161543 ) ) ;
#8829 = EDGE_CURVE ( 'NONE', #10056, #6004, #14776, .T. ) ;
#8830 = VERTEX_POINT ( 'NONE', #10089 ) ;
#8831 = VECTOR ( 'NONE', #9832, 1000.000000000000000 ) ;
#8832 = CARTESIAN_POINT ( 'NONE',  ( 0.02436607992776411782, -24.63872515616084513, 2.336989772644183283 ) ) ;
#8833 = CYLINDRICAL_SURFACE ( 'NONE', #2422, 5.700000000000001954 ) ;
#8834 = CARTESIAN_POINT ( 'NONE',  ( 12.34374999795161543, -3.114526743279282250, 3.846120219227923798 ) ) ;
#8835 = AXIS2_PLACEMENT_3D ( 'NONE', #11115, #18516, #6588 ) ;
#8836 = ORIENTED_EDGE ( 'NONE', *, *, #2536, .T. ) ;
#8837 = DIRECTION ( 'NONE',  ( -1.000000000000000000, 0.000000000000000000, -0.000000000000000000 ) ) ;
#8838 = VERTEX_POINT ( 'NONE', #7047 ) ;
#8839 = CARTESIAN_POINT ( 'NONE',  ( 0.5279273381794601372, -26.82026385750175734, -3.461047254864539457 ) ) ;
#8840 = ORIENTED_EDGE ( 'NONE', *, *, #2897, .T. ) ;
#8841 = LINE ( 'NONE', #2823, #8618 ) ;
#8842 = DIRECTION ( 'NONE',  ( 0.8191520442889898002, 0.000000000000000000, 0.5735764363510488240 ) ) ;
#8843 = EDGE_CURVE ( 'NONE', #2115, #1752, #17650, .T. ) ;
#8844 = CARTESIAN_POINT ( 'NONE',  ( -3.954556930911881096, -2.873153789725797935, -14.84374999795161543 ) ) ;
#8845 = CARTESIAN_POINT ( 'NONE',  ( 11.96874999795161365, -1.773574444220693325, -4.620319390059841602 ) ) ;
#8846 = DIRECTION ( 'NONE',  ( 1.000000000000000000, 0.000000000000000000, 0.000000000000000000 ) ) ;
#8847 = ORIENTED_EDGE ( 'NONE', *, *, #2197, .F. ) ;
#8848 = DIRECTION ( 'NONE',  ( 0.000000000000000000, 0.000000000000000000, 1.000000000000000000 ) ) ;
#8849 = ADVANCED_FACE ( 'NONE', ( #5660 ), #2558, .F. ) ;
#8850 = AXIS2_PLACEMENT_3D ( 'NONE', #98, #1701, #17104 ) ;
#8852 = EDGE_CURVE ( 'NONE', #8225, #12806, #12854, .T. ) ;
#8851 = EDGE_CURVE ( 'NONE', #17102, #2419, #8051, .T. ) ;
#8853 = AXIS2_PLACEMENT_3D ( 'NONE', #16524, #4610, #2799 ) ;
#8854 = VERTEX_POINT ( 'NONE', #10181 ) ;
#8855 = CARTESIAN_POINT ( 'NONE',  ( -4.762500000000000178, 0.000000000000000000, -6.502399999999998847 ) ) ;
#8856 = DIRECTION ( 'NONE',  ( -0.000000000000000000, 0.000000000000000000, 1.000000000000000000 ) ) ;
#8857 = DIRECTION ( 'NONE',  ( 0.000000000000000000, 0.000000000000000000, 1.000000000000000000 ) ) ;
#8858 = DIRECTION ( 'NONE',  ( -1.000000000000000000, -0.000000000000000000, -0.000000000000000000 ) ) ;
#8859 = VERTEX_POINT ( 'NONE', #16377 ) ;
#8860 =( BOUNDED_SURFACE ( )  B_SPLINE_SURFACE ( 1, 2, ( 
 ( #16184, #6551, #5364, #8374, #10083, #16084, #17481, #12781, #2455, #3669, #12683, #9791, #11570, #5458, #11477, #18879, #5067 ),
 ( #14177, #17577, #18774, #8272, #9984, #9690, #14380, #3770, #14490, #6852, #15885, #3865, #11180, #480, #15783, #678, #12880 ) ),
 .UNSPECIFIED., .F., .F., .F. ) 
 B_SPLINE_SURFACE_WITH_KNOTS ( ( 2, 2 ),
 ( 3, 2, 2, 2, 2, 2, 2, 2, 3 ),
 ( 0.000000000000000000, 1.000000000000000000 ),
 ( 0.000000000000000000, 0.05000000000000000278, 0.1000000000000000056, 0.1499999999999999944, 0.2000000000000000111, 0.2500000000000000000, 0.2999999999999999889, 0.3499999999999999778, 0.4000000000000000222 ),
 .UNSPECIFIED. ) 
 GEOMETRIC_REPRESENTATION_ITEM ( )  RATIONAL_B_SPLINE_SURFACE ( (
 ( 1.000000000000000000, 0.9876883405951377704, 1.000000000000000000, 0.9876883405951377704, 1.000000000000000000, 0.9876883405951377704, 1.000000000000000000, 0.9876883405951377704, 1.000000000000000000, 0.9876883405951377704, 1.000000000000000000, 0.9876883405951377704, 1.000000000000000000, 0.9876883405951377704, 1.000000000000000000, 0.9876883405951377704, 1.000000000000000000),
 ( 1.000000000000000000, 0.9876883405951377704, 1.000000000000000000, 0.9876883405951377704, 1.000000000000000000, 0.9876883405951377704, 1.000000000000000000, 0.9876883405951377704, 1.000000000000000000, 0.9876883405951377704, 1.000000000000000000, 0.9876883405951377704, 1.000000000000000000, 0.9876883405951377704, 1.000000000000000000, 0.9876883405951377704, 1.000000000000000000) ) ) 
 REPRESENTATION_ITEM ( '' )  SURFACE ( )  );
#8861 = DIRECTION ( 'NONE',  ( -1.000000000000000000, 0.000000000000000000, 0.000000000000000000 ) ) ;
#8862 = CIRCLE ( 'NONE', #15255, 4.200000000000000178 ) ;
#8863 = DIRECTION ( 'NONE',  ( 0.000000000000000000, 0.000000000000000000, 1.000000000000000000 ) ) ;
#8864 = CARTESIAN_POINT ( 'NONE',  ( 13.00000000000000533, 4.611396867937201272, 3.350375938067096548 ) ) ;
#8865 = VECTOR ( 'NONE', #10448, 1000.000000000000000 ) ;
#8866 =( NAMED_UNIT ( * ) SI_UNIT ( $, .STERADIAN. ) SOLID_ANGLE_UNIT ( ) );
#8867 = EDGE_LOOP ( 'NONE', ( #13414, #16218, #17420, #6447 ) ) ;
#8868 = ORIENTED_EDGE ( 'NONE', *, *, #13771, .T. ) ;
#8869 = DIRECTION ( 'NONE',  ( 1.000000000000000000, 0.000000000000000000, 0.000000000000000000 ) ) ;
#8870 = CYLINDRICAL_SURFACE ( 'NONE', #6614, 1.000000000000004441 ) ;
#8871 = ORIENTED_EDGE ( 'NONE', *, *, #8375, .T. ) ;
#8872 = DIRECTION ( 'NONE',  ( 0.000000000000000000, 0.000000000000000000, -1.000000000000000000 ) ) ;
#8873 = ORIENTED_EDGE ( 'NONE', *, *, #15833, .T. ) ;
#8874 = FACE_OUTER_BOUND ( 'NONE', #6329, .T. ) ;
#8875 = CARTESIAN_POINT ( 'NONE',  ( 9.603018496175287840E-16, -5.456805104200934231, -23.69843731927176123 ) ) ;
#8876 = VECTOR ( 'NONE', #7593, 1000.000000000000000 ) ;
#8877 = VERTEX_POINT ( 'NONE', #13368 ) ;
#8878 = VECTOR ( 'NONE', #7725, 1000.000000000000000 ) ;
#8879 = CARTESIAN_POINT ( 'NONE',  ( 2.790000000000076419, 9.515416771311512534, -22.38018801136466251 ) ) ;
#8880 = CYLINDRICAL_SURFACE ( 'NONE', #9088, 2.524999999999995914 ) ;
#8881 = CARTESIAN_POINT ( 'NONE',  ( -0.9027913098498963063, -5.699999999999994849, -12.81249999590322552 ) ) ;
#8882 = ORIENTED_EDGE ( 'NONE', *, *, #16191, .F. ) ;
#8883 = DIRECTION ( 'NONE',  ( -1.000000000000000000, -0.000000000000000000, 0.000000000000000000 ) ) ;
#8884 = SHAPE_REPRESENTATION_RELATIONSHIP ( 'NONE' , 'NONE' ,  #17568, #4233 ) ;
#8885 = CARTESIAN_POINT ( 'NONE',  ( 0.006974693931642682830, -16.17543236987975064, -18.43727551351049598 ) ) ;
#8886 = EDGE_LOOP ( 'NONE', ( #8543, #10861, #4909, #5614 ) ) ;
#8887 = DIRECTION ( 'NONE',  ( -1.000000000000000000, 0.000000000000000000, 0.000000000000000000 ) ) ;
#8888 = AXIS2_PLACEMENT_3D ( 'NONE', #1087, #10295, #8887 ) ;
#8889 = FACE_BOUND ( 'NONE', #17563, .T. ) ;
#8890 = CARTESIAN_POINT ( 'NONE',  ( 5.700000000000001954, 0.000000000000000000, 0.000000000000000000 ) ) ;
#8891 = AXIS2_PLACEMENT_3D ( 'NONE', #12393, #14283, #17385 ) ;
#8892 = CARTESIAN_POINT ( 'NONE',  ( 3.631935042553954940, -7.068536848887564616, -2.426114119173129746E-15 ) ) ;
#8893 = CARTESIAN_POINT ( 'NONE',  ( -4.235925505221191933, -3.814044456245443193, -8.312499995903225525 ) ) ;
#8894 = ADVANCED_FACE ( 'NONE', ( #7244 ), #7345, .F. ) ;
#8895 = ORIENTED_EDGE ( 'NONE', *, *, #7722, .T. ) ;
#8896 = FACE_OUTER_BOUND ( 'NONE', #4854, .T. ) ;
#8897 = CARTESIAN_POINT ( 'NONE',  ( -4.780397808154273953, -1.280903732194386579, -8.968749997951613651 ) ) ;
#8898 = ORIENTED_EDGE ( 'NONE', *, *, #19711, .F. ) ;
#8899 = CARTESIAN_POINT ( 'NONE',  ( 14.84374999795161543, -4.861323657744410554, 0.5109457054261454800 ) ) ;
#8900 = DIRECTION ( 'NONE',  ( -0.9773501006361902110, 2.591706245282799409E-17, -0.2116288751244233268 ) ) ;
#8901 = AXIS2_PLACEMENT_3D ( 'NONE', #17771, #19460, #5747 ) ;
#8902 = CARTESIAN_POINT ( 'NONE',  ( 9.671566133830877376, 15.77352024078954784, 32.00000000000000000 ) ) ;
#8903 = CARTESIAN_POINT ( 'NONE',  ( -0.6492350739117196401, -8.790599478695048319, -0.4925372136696601344 ) ) ;
#8904 = EDGE_LOOP ( 'NONE', ( #15073, #12913, #4012, #6851 ) ) ;
#8905 = CARTESIAN_POINT ( 'NONE',  ( 10.46874999795161720, 4.648860486681953397, -1.510506337161861667 ) ) ;
#8906 = FILL_AREA_STYLE_COLOUR ( '', #19597 ) ;
#8907 = CARTESIAN_POINT ( 'NONE',  ( -30.00000000000000000, -4.200000000000000178, 0.000000000000000000 ) ) ;
#8908 = ADVANCED_FACE ( 'NONE', ( #16482 ), #8971, .T. ) ;
#8909 = DIRECTION ( 'NONE',  ( 1.000000000000000000, 0.000000000000000000, 0.000000000000000000 ) ) ;
#8910 = ORIENTED_EDGE ( 'NONE', *, *, #547, .F. ) ;
#8911 = CARTESIAN_POINT ( 'NONE',  ( 0.07186814640506923590, 12.74240566898984284, 21.92302674874967749 ) ) ;
#8912 = ORIENTED_EDGE ( 'NONE', *, *, #1981, .F. ) ;
#8913 = CARTESIAN_POINT ( 'NONE',  ( 15.28688694438835505, -7.664027248171309203, -32.00000000000000000 ) ) ;
#8914 = CARTESIAN_POINT ( 'NONE',  ( -41.99999999999999289, 4.399999999999997691, 0.000000000000000000 ) ) ;
#8915 = LINE ( 'NONE', #15417, #9344 ) ;
#8916 = AXIS2_PLACEMENT_3D ( 'NONE', #11205, #12708, #12145 ) ;
#8917 = PLANE ( 'NONE',  #16553 ) ;
#8918 = EDGE_CURVE ( 'NONE', #16209, #5291, #8573, .T. ) ;
#8919 = VERTEX_POINT ( 'NONE', #5754 ) ;
#8920 = CARTESIAN_POINT ( 'NONE',  ( 2.604434404052933694, 17.45907811351455408, 19.17825124759784572 ) ) ;
#8921 = CARTESIAN_POINT ( 'NONE',  ( 2.789999999999999147, -15.74360496233368245, -18.28042085475295409 ) ) ;
#8922 = ORIENTED_EDGE ( 'NONE', *, *, #7632, .T. ) ;
#8923 = AXIS2_PLACEMENT_3D ( 'NONE', #7436, #2745, #18169 ) ;
#8924 = DIRECTION ( 'NONE',  ( -1.000000000000000000, -0.000000000000000000, -0.000000000000000000 ) ) ;
#8925 = CARTESIAN_POINT ( 'NONE',  ( -2.873153789725852558, -3.954556930911842016, -13.84374999795161543 ) ) ;
#8926 = VECTOR ( 'NONE', #6783, 1000.000000000000000 ) ;
#8927 = VERTEX_POINT ( 'NONE', #15074 ) ;
#8928 = CARTESIAN_POINT ( 'NONE',  ( 4.233219804643887585, 2.444050593749990785, -11.84374999795161365 ) ) ;
#8929 = CARTESIAN_POINT ( 'NONE',  ( 9.812499995903223748, 5.574407415329156734, 1.493657965219523875 ) ) ;
#8930 = CARTESIAN_POINT ( 'NONE',  ( -2.000000000000000888, 5.143516556418882928E-16, 4.200000000000000178 ) ) ;
#8931 = VERTEX_POINT ( 'NONE', #16281 ) ;
#8932 = EDGE_CURVE ( 'NONE', #14603, #2736, #2938, .T. ) ;
#8933 = LINE ( 'NONE', #15036, #19479 ) ;
#8934 = ORIENTED_EDGE ( 'NONE', *, *, #6483, .T. ) ;
#8935 = EDGE_CURVE ( 'NONE', #1705, #993, #18079, .T. ) ;
#8936 = DIRECTION ( 'NONE',  ( 0.000000000000000000, 0.000000000000000000, 1.000000000000000000 ) ) ;
#8937 = ORIENTED_EDGE ( 'NONE', *, *, #2557, .T. ) ;
#8938 = AXIS2_PLACEMENT_3D ( 'NONE', #17402, #15903, #11860 ) ;
#8939 = DIRECTION ( 'NONE',  ( -0.000000000000000000, -0.000000000000000000, -1.000000000000000000 ) ) ;
#8940 = CARTESIAN_POINT ( 'NONE',  ( 3.889375000000000693, 0.000000000000000000, -0.6113687067993561763 ) ) ;
#8941 = CARTESIAN_POINT ( 'NONE',  ( -1.510506337161893642, -4.648860486681943627, -12.84374999795161543 ) ) ;
#8942 = CARTESIAN_POINT ( 'NONE',  ( 1.749999999999998002, -4.147968289691484678, 27.76164181293050603 ) ) ;
#8943 = EDGE_CURVE ( 'NONE', #3123, #2987, #4221, .T. ) ;
#8944 = ORIENTED_EDGE ( 'NONE', *, *, #17472, .T. ) ;
#8945 = CARTESIAN_POINT ( 'NONE',  ( 1.749999999999998002, 25.12109765559653596, 12.52377138324232675 ) ) ;
#8946 = ADVANCED_FACE ( 'NONE', ( #8874 ), #13179, .T. ) ;
#8947 = FACE_OUTER_BOUND ( 'NONE', #14534, .T. ) ;
#8948 = EDGE_LOOP ( 'NONE', ( #7218, #10893 ) ) ;
#8949 = CARTESIAN_POINT ( 'NONE',  ( 2.999999999999998224, 3.218695387886217230, -3.000000000000000000 ) ) ;
#8950 = EDGE_CURVE ( 'NONE', #10504, #12259, #11711, .T. ) ;
#8951 = DIRECTION ( 'NONE',  ( 1.000000000000000000, 0.000000000000000000, 0.000000000000000000 ) ) ;
#8952 = ORIENTED_EDGE ( 'NONE', *, *, #11176, .T. ) ;
#8953 = CARTESIAN_POINT ( 'NONE',  ( 0.6764999999999817826, 4.898587196589412829E-16, -4.000000000000000000 ) ) ;
#8954 = CARTESIAN_POINT ( 'NONE',  ( 112.0000000000000000, 0.000000000000000000, 0.000000000000000000 ) ) ;
#8955 = DIRECTION ( 'NONE',  ( -1.000000000000000000, -0.000000000000000000, -0.000000000000000000 ) ) ;
#8956 = EDGE_LOOP ( 'NONE', ( #971, #10661 ) ) ;
#8957 = CARTESIAN_POINT ( 'NONE',  ( 2.695436003842732298, 4.150607464521791634, -9.968749997951615427 ) ) ;
#8958 = VERTEX_POINT ( 'NONE', #4072 ) ;
#8959 = DIRECTION ( 'NONE',  ( -0.06085899303095324009, -0.9981463735180619024, 0.000000000000000000 ) ) ;
#8960 = EDGE_CURVE ( 'NONE', #600, #15138, #4270, .T. ) ;
#8961 = CARTESIAN_POINT ( 'NONE',  ( 1.749999999999998002, -4.633866840648726004, -27.68468304288263582 ) ) ;
#8962 = VERTEX_POINT ( 'NONE', #19369 ) ;
#8963 = VERTEX_POINT ( 'NONE', #4168 ) ;
#8964 = DIRECTION ( 'NONE',  ( -0.000000000000000000, -0.000000000000000000, 1.000000000000000000 ) ) ;
#8965 = VECTOR ( 'NONE', #10264, 1000.000000000000000 ) ;
#8966 = CARTESIAN_POINT ( 'NONE',  ( -18.68117051311639543, -3.372863662543042818, 32.00000000000000000 ) ) ;
#8967 = AXIS2_PLACEMENT_3D ( 'NONE', #7988, #394, #6474 ) ;
#8968 = ORIENTED_EDGE ( 'NONE', *, *, #15427, .T. ) ;
#8969 = CARTESIAN_POINT ( 'NONE',  ( 2.500000000000002220, 0.000000000000000000, 0.000000000000000000 ) ) ;
#8970 = ORIENTED_EDGE ( 'NONE', *, *, #1397, .T. ) ;
#8971 = CYLINDRICAL_SURFACE ( 'NONE', #19238, 28.06981291497571362 ) ;
#8972 = CARTESIAN_POINT ( 'NONE',  ( 0.000000000000000000, 0.000000000000000000, 0.000000000000000000 ) ) ;
#8973 = ORIENTED_EDGE ( 'NONE', *, *, #8822, .F. ) ;
#8974 = EDGE_CURVE ( 'NONE', #4210, #5957, #9676, .T. ) ;
#8975 =( BOUNDED_CURVE ( )  B_SPLINE_CURVE ( 2, ( #8396, #5290, #11198, #14298, #1160, #14402, #3689, #6573, #7234, #18796, #8192, #3592, #6871, #18997, #8089 ),
 .UNSPECIFIED., .F., .F. ) 
 B_SPLINE_CURVE_WITH_KNOTS ( ( 3, 2, 2, 2, 2, 2, 2, 3 ),
 ( 0.000000000000000000, 0.05000000000000000971, 0.1000000000000000194, 0.1499999999999999944, 0.2000000000000000389, 0.2500000000000000000, 0.2999999999999999889, 0.3333180920165872418 ),
 .UNSPECIFIED. ) 
 CURVE ( )  GEOMETRIC_REPRESENTATION_ITEM ( )  RATIONAL_B_SPLINE_CURVE ( ( 1.000000000000000000, 0.9876883405951377704, 1.000000000000000000, 0.9876883405951377704, 1.000000000000000000, 0.9876883405951377704, 1.000000000000000000, 0.9876883405951377704, 1.000000000000000000, 0.9876883405951377704, 1.000000000000000000, 0.9876883405951377704, 1.000000000000000000, 0.9917959799814383137, 0.9945256517182510247 ) ) 
 REPRESENTATION_ITEM ( '' )  );
#8976 = PLANE ( 'NONE',  #3608 ) ;
#8977 = CARTESIAN_POINT ( 'NONE',  ( -7.288264926088305451, 4.957553806382917649, -0.4925372136696566372 ) ) ;
#8978 = CARTESIAN_POINT ( 'NONE',  ( -0.5109457054261112852, 4.861323657744413218, -14.46874999795161720 ) ) ;
#8979 = EDGE_CURVE ( 'NONE', #9207, #10781, #17984, .T. ) ;
#8980 = ORIENTED_EDGE ( 'NONE', *, *, #4030, .T. ) ;
#8981 = LINE ( 'NONE', #15086, #17147 ) ;
#8982 =( NAMED_UNIT ( * ) PLANE_ANGLE_UNIT ( ) SI_UNIT ( $, .RADIAN. ) );
#8983 = EDGE_CURVE ( 'NONE', #11811, #16968, #17008, .T. ) ;
#8984 = CARTESIAN_POINT ( 'NONE',  ( 0.9659243001600011924, 24.74770846292485516, 12.96726489871199028 ) ) ;
#8985 = ORIENTED_EDGE ( 'NONE', *, *, #14235, .T. ) ;
#8986 = DIRECTION ( 'NONE',  ( 0.000000000000000000, 0.000000000000000000, -1.000000000000000000 ) ) ;
#8987 = FACE_BOUND ( 'NONE', #16703, .T. ) ;
#8988 = PRODUCT_DEFINITION_CONTEXT ( 'detailed design', #11110, 'design' ) ;
#8989 = CARTESIAN_POINT ( 'NONE',  ( -30.00000000000000000, -4.400000000000000355, 5.388445916248354013E-16 ) ) ;
#8990 = CARTESIAN_POINT ( 'NONE',  ( 4.620319390059819398, -1.773574444220757496, -10.96874999795161720 ) ) ;
#8991 = CARTESIAN_POINT ( 'NONE',  ( 1.039999999999996483, -27.76164181293054511, 4.147968289691193355 ) ) ;
#8992 = CIRCLE ( 'NONE', #1958, 1.000000000000000888 ) ;
#8993 = ORIENTED_EDGE ( 'NONE', *, *, #1510, .T. ) ;
#8994 = CARTESIAN_POINT ( 'NONE',  ( 2.765633920072235519, -18.55949924794880346, -16.37294372382878649 ) ) ;
#8995 = AXIS2_PLACEMENT_3D ( 'NONE', #14562, #6930, #5439 ) ;
#8996 = CARTESIAN_POINT ( 'NONE',  ( -4.861323657744413218, -0.5109457054261099529, -9.468749997951615427 ) ) ;
#8997 = ORIENTED_EDGE ( 'NONE', *, *, #16277, .T. ) ;
#8998 = B_SPLINE_CURVE_WITH_KNOTS ( 'NONE', 3,
 ( #8388, #18991, #691, #6769, #12893, #5282 ),
 .UNSPECIFIED., .F., .F.,
 ( 4, 2, 4 ),
 ( 2.321268216997177022E-07, 0.001878622960950496190, 0.003757013795079292354 ),
 .UNSPECIFIED. ) ;
#8999 = CARTESIAN_POINT ( 'NONE',  ( 13.34374999795161365, -4.150607464521812062, 2.695436003842704764 ) ) ;
#9000 = ADVANCED_FACE ( 'NONE', ( #18466 ), #9074, .F. ) ;
#9001 = LINE ( 'NONE', #2786, #10892 ) ;
#9002 = CARTESIAN_POINT ( 'NONE',  ( -11.32184790671638730, 13.12143529358541549, -32.00000000000000000 ) ) ;
#9003 = DIRECTION ( 'NONE',  ( 1.000000000000000000, 0.000000000000000000, 0.000000000000000000 ) ) ;
#9004 = EDGE_LOOP ( 'NONE', ( #9026, #16691 ) ) ;
#9005 = CARTESIAN_POINT ( 'NONE',  ( 0.000000000000000000, 0.000000000000000000, 0.000000000000000000 ) ) ;
#9006 = PRESENTATION_STYLE_ASSIGNMENT (( #6086 ) ) ;
#9007 = CARTESIAN_POINT ( 'NONE',  ( 1.039999999999996705, 19.67366047555530173, 20.02152543075352398 ) ) ;
#9008 = ADVANCED_FACE ( 'NONE', ( #1565 ), #164, .T. ) ;
#9009 = CYLINDRICAL_SURFACE ( 'NONE', #10879, 1.000000000000005995 ) ;
#9010 = VERTEX_POINT ( 'NONE', #13873 ) ;
#9011 = CARTESIAN_POINT ( 'NONE',  ( 5.626241948324195441, -16.73597674598852691, 35.00000000000000000 ) ) ;
#9012 = CARTESIAN_POINT ( 'NONE',  ( 2.790000000000000036, -20.65025570340076655, -12.51972505885016140 ) ) ;
#9013 = FACE_OUTER_BOUND ( 'NONE', #2759, .T. ) ;
#9014 = LINE ( 'NONE', #16426, #16997 ) ;
#9015 = EDGE_CURVE ( 'NONE', #11304, #13799, #12076, .T. ) ;
#9016 = CARTESIAN_POINT ( 'NONE',  ( 2.789999999999999147, 7.909232158575156824, -24.34211360614291664 ) ) ;
#9017 = ORIENTED_EDGE ( 'NONE', *, *, #16236, .T. ) ;
#9018 = CARTESIAN_POINT ( 'NONE',  ( 2.031033479673589159, 19.12621924769867121, 19.86422722021319487 ) ) ;
#9019 = LINE ( 'NONE', #2807, #6889 ) ;
#9020 = CIRCLE ( 'NONE', #18911, 5.700000000000001954 ) ;
#9021 = EDGE_LOOP ( 'NONE', ( #16987, #8033, #2619, #15310 ) ) ;
#9022 = AXIS2_PLACEMENT_3D ( 'NONE', #18883, #11287, #15686 ) ;
#9023 = AXIS2_PLACEMENT_3D ( 'NONE', #12606, #3687, #17401 ) ;
#9024 = CARTESIAN_POINT ( 'NONE',  ( -2.993098736590125853E-16, 4.888101187500000222, -11.84374999795161365 ) ) ;
#9025 = CARTESIAN_POINT ( 'NONE',  ( -0.7741991708319226895, -4.888101187499994893, -12.34374999795161543 ) ) ;
#9026 = ORIENTED_EDGE ( 'NONE', *, *, #17752, .T. ) ;
#9027 = DIRECTION ( 'NONE',  ( 1.000000000000000000, 0.000000000000000000, 0.000000000000000000 ) ) ;
#9028 = CARTESIAN_POINT ( 'NONE',  ( 10.31249999590322552, 5.207209108562820710, 2.318398865532073749 ) ) ;
#9029 = CARTESIAN_POINT ( 'NONE',  ( 0.07186808533286681566, 23.19485392143213431, 10.24630254990524314 ) ) ;
#9030 = EDGE_CURVE ( 'NONE', #10900, #3614, #1987, .T. ) ;
#9031 = ORIENTED_EDGE ( 'NONE', *, *, #3106, .F. ) ;
#9032 = CYLINDRICAL_SURFACE ( 'NONE', #14383, 13.19999999999999929 ) ;
#9033 = ORIENTED_EDGE ( 'NONE', *, *, #8236, .T. ) ;
#9034 = FACE_OUTER_BOUND ( 'NONE', #1815, .T. ) ;
#9035 = AXIS2_PLACEMENT_3D ( 'NONE', #13067, #2160, #670 ) ;
#9036 = ORIENTED_EDGE ( 'NONE', *, *, #7465, .T. ) ;
#9037 = AXIS2_PLACEMENT_3D ( 'NONE', #15351, #4831, #18346 ) ;
#9038 = CARTESIAN_POINT ( 'NONE',  ( -39.64101615137792578, 82.80384757729314060, 41.99999999999999289 ) ) ;
#9039 = CARTESIAN_POINT ( 'NONE',  ( 1.039999999999994929, -25.12109765559662833, 12.52377138324214023 ) ) ;
#9040 = CARTESIAN_POINT ( 'NONE',  ( 13.96874999795161365, 1.280903732194486722, -4.780397808154247308 ) ) ;
#9041 = VECTOR ( 'NONE', #19039, 1000.000000000000000 ) ;
#9042 = DIRECTION ( 'NONE',  ( 1.000000000000000000, 1.224646799147353207E-16, -0.000000000000000000 ) ) ;
#9043 = ORIENTED_EDGE ( 'NONE', *, *, #14663, .T. ) ;
#9044 = MECHANICAL_DESIGN_GEOMETRIC_PRESENTATION_REPRESENTATION (  '', ( #9681 ), #3598 ) ;
#9045 = CYLINDRICAL_SURFACE ( 'NONE', #12190, 5.700000000000001954 ) ;
#9046 = ADVANCED_FACE ( 'NONE', ( #18275 ), #18564, .F. ) ;
#9047 = SURFACE_SIDE_STYLE ('',( #36 ) ) ;
#9048 = EDGE_CURVE ( 'NONE', #14720, #4121, #3903, .T. ) ;
#9049 = EDGE_CURVE ( 'NONE', #17165, #19497, #15406, .T. ) ;
#9050 = AXIS2_PLACEMENT_3D ( 'NONE', #19750, #15058, #5739 ) ;
#9051 = ORIENTED_EDGE ( 'NONE', *, *, #7675, .F. ) ;
#9052 = DIRECTION ( 'NONE',  ( 0.000000000000000000, 0.000000000000000000, 1.000000000000000000 ) ) ;
#9053 = LINE ( 'NONE', #15153, #17667 ) ;
#9054 = ORIENTED_EDGE ( 'NONE', *, *, #1303, .T. ) ;
#9055 = DIRECTION ( 'NONE',  ( -1.000000000000000000, 0.000000000000000000, 0.000000000000000000 ) ) ;
#9056 = CARTESIAN_POINT ( 'NONE',  ( -2.500000000000002220, 0.000000000000000000, 0.000000000000000000 ) ) ;
#9057 = EDGE_CURVE ( 'NONE', #17114, #1278, #4564, .T. ) ;
#9058 = CARTESIAN_POINT ( 'NONE',  ( 9.000000000000000000, 0.000000000000000000, 35.00000000000000000 ) ) ;
#9059 = VERTEX_POINT ( 'NONE', #10769 ) ;
#9060 = CARTESIAN_POINT ( 'NONE',  ( 4.620319390059829168, 1.773574444220725299, -11.96874999795161365 ) ) ;
#9061 = VERTEX_POINT ( 'NONE', #18181 ) ;
#9062 = DIRECTION ( 'NONE',  ( -0.06941516925093198231, -0.9975878579242355437, -5.779973937047467298E-18 ) ) ;
#9063 = DIRECTION ( 'NONE',  ( 0.000000000000000000, 0.000000000000000000, 1.000000000000000000 ) ) ;
#9064 = DIRECTION ( 'NONE',  ( 4.060088635510494296E-15, -1.000000000000000000, 0.000000000000000000 ) ) ;
#9065 = ORIENTED_EDGE ( 'NONE', *, *, #10561, .F. ) ;
#9066 = VERTEX_POINT ( 'NONE', #9372 ) ;
#9067 = DIRECTION ( 'NONE',  ( 0.000000000000000000, 0.000000000000000000, 1.000000000000000000 ) ) ;
#9068 = STYLED_ITEM ( 'NONE', ( #9006 ), #19745 ) ;
#9069 = APPLICATION_CONTEXT ( 'automotive_design' ) ;
#9070 = CARTESIAN_POINT ( 'NONE',  ( 2.718131864678289933, -2.577209017046833583, -25.22589920183363787 ) ) ;
#9071 = EDGE_LOOP ( 'NONE', ( #7538, #4933, #19684, #13761 ) ) ;
#9072 = CARTESIAN_POINT ( 'NONE',  ( -19.00000000000000355, 1.224646799147353207E-16, 0.000000000000000000 ) ) ;
#9073 = ORIENTED_EDGE ( 'NONE', *, *, #1840, .F. ) ;
#9074 = CYLINDRICAL_SURFACE ( 'NONE', #12541, 1.000000000000002665 ) ;
#9075 = TOROIDAL_SURFACE ( 'NONE', #15459, 24.12539914357697413, 8.000000000000000000 ) ;
#9076 = PRODUCT_DEFINITION ( 'UNKNOWN', '', #3478, #8988 ) ;
#9077 = ORIENTED_EDGE ( 'NONE', *, *, #10170, .F. ) ;
#9078 = COLOUR_RGB ( '', 0.09019608, 0.27058824, 0.51372549) ;
#9079 = AXIS2_PLACEMENT_3D ( 'NONE', #4572, #16884, #3165 ) ;
#9080 = EDGE_CURVE ( 'NONE', #3395, #19037, #4544, .T. ) ;
#9081 = FACE_OUTER_BOUND ( 'NONE', #406, .T. ) ;
#9082 = CARTESIAN_POINT ( 'NONE',  ( 13.81249999590322552, 5.142044285764750811, 2.620002426024544029 ) ) ;
#9083 = DIRECTION ( 'NONE',  ( 0.000000000000000000, 0.7315216790650488354, 0.6818181818181822118 ) ) ;
#9084 = EDGE_CURVE ( 'NONE', #16572, #2028, #15375, .T. ) ;
#9085 = ORIENTED_EDGE ( 'NONE', *, *, #13512, .F. ) ;
#9086 = CARTESIAN_POINT ( 'NONE',  ( 1.749999999999998002, 0.000000000000000000, 0.000000000000000000 ) ) ;
#9087 = CARTESIAN_POINT ( 'NONE',  ( -36.00000000000000000, 6.000000000000000888, 0.000000000000000000 ) ) ;
#9088 = AXIS2_PLACEMENT_3D ( 'NONE', #14981, #67, #4669 ) ;
#9089 = ORIENTED_EDGE ( 'NONE', *, *, #16757, .T. ) ;
#9090 = DIRECTION ( 'NONE',  ( -0.000000000000000000, -0.000000000000000000, -1.000000000000000000 ) ) ;
#9091 = CARTESIAN_POINT ( 'NONE',  ( 1.394999999999999574, 19.67366047555530528, 20.02152543075352753 ) ) ;
#9092 = CARTESIAN_POINT ( 'NONE',  ( 1.255998204157470211, -17.85806462366060288, -32.00000000000000000 ) ) ;
#9093 = EDGE_CURVE ( 'NONE', #1584, #8643, #1682, .T. ) ;
#9094 = DIRECTION ( 'NONE',  ( 1.000000000000000000, 0.000000000000000000, 0.000000000000000000 ) ) ;
#9095 = CARTESIAN_POINT ( 'NONE',  ( 3.499494075959815653, 3.499494075959816541, -14.34374999795161365 ) ) ;
#9096 = ORIENTED_EDGE ( 'NONE', *, *, #1104, .T. ) ;
#9097 = FACE_BOUND ( 'NONE', #19257, .T. ) ;
#9098 =( BOUNDED_SURFACE ( )  B_SPLINE_SURFACE ( 1, 2, ( 
 ( #2211, #624, #19210, #12728, #18824, #12925, #3617, #5107, #6701, #19023, #11333, #17431, #15928, #11427, #17527, #3814, #2794 ),
 ( #18022, #7184, #18114, #7086, #16611, #16316, #5694, #5896, #1110, #13306, #5597, #10610, #12112, #11709, #4207, #15012, #4403 ) ),
 .UNSPECIFIED., .F., .F., .F. ) 
 B_SPLINE_SURFACE_WITH_KNOTS ( ( 2, 2 ),
 ( 3, 2, 2, 2, 2, 2, 2, 2, 3 ),
 ( 0.000000000000000000, 1.000000000000000000 ),
 ( 0.000000000000000000, 0.05000000000000000278, 0.1000000000000000056, 0.1499999999999999944, 0.2000000000000000111, 0.2500000000000000000, 0.2999999999999999889, 0.3499999999999999778, 0.4000000000000000222 ),
 .UNSPECIFIED. ) 
 GEOMETRIC_REPRESENTATION_ITEM ( )  RATIONAL_B_SPLINE_SURFACE ( (
 ( 1.000000000000000000, 0.9876883405951377704, 1.000000000000000000, 0.9876883405951377704, 1.000000000000000000, 0.9876883405951377704, 1.000000000000000000, 0.9876883405951377704, 1.000000000000000000, 0.9876883405951377704, 1.000000000000000000, 0.9876883405951377704, 1.000000000000000000, 0.9876883405951377704, 1.000000000000000000, 0.9876883405951377704, 1.000000000000000000),
 ( 1.000000000000000000, 0.9876883405951377704, 1.000000000000000000, 0.9876883405951377704, 1.000000000000000000, 0.9876883405951377704, 1.000000000000000000, 0.9876883405951377704, 1.000000000000000000, 0.9876883405951377704, 1.000000000000000000, 0.9876883405951377704, 1.000000000000000000, 0.9876883405951377704, 1.000000000000000000, 0.9876883405951377704, 1.000000000000000000) ) ) 
 REPRESENTATION_ITEM ( '' )  SURFACE ( )  );
#9099 = DIRECTION ( 'NONE',  ( -1.000000000000000000, -0.000000000000000000, -0.000000000000000000 ) ) ;
#9100 = EDGE_CURVE ( 'NONE', #4315, #15354, #4237, .T. ) ;
#9101 = ORIENTED_EDGE ( 'NONE', *, *, #18788, .F. ) ;
#9102 = CARTESIAN_POINT ( 'NONE',  ( 10.34374999795161543, -0.2590123213421313686, 4.942249507334556036 ) ) ;
#9103 = EDGE_CURVE ( 'NONE', #3073, #13634, #17024, .T. ) ;
#9104 = CIRCLE ( 'NONE', #5886, 1.000000000000004441 ) ;
#9105 = CARTESIAN_POINT ( 'NONE',  ( 7.312499995903225525, -4.936344801571327601, 2.849999999999954348 ) ) ;
#9106 = CARTESIAN_POINT ( 'NONE',  ( 5.510910596163084625E-16, 18.00000000000000355, 32.00000000000000000 ) ) ;
#9107 = CARTESIAN_POINT ( 'NONE',  ( 7.000000000000005329, 5.575441324182695446, -1.185096637661215091 ) ) ;
#9108 = VERTEX_POINT ( 'NONE', #6054 ) ;
#9109 = AXIS2_PLACEMENT_3D ( 'NONE', #2488, #16121, #17611 ) ;
#9110 = LINE ( 'NONE', #4450, #2064 ) ;
#9111 = DIRECTION ( 'NONE',  ( 0.9773501006361904331, 2.591706245282795403E-17, 0.2116288751244229938 ) ) ;
#9112 = ORIENTED_EDGE ( 'NONE', *, *, #6193, .F. ) ;
#9113 = LINE ( 'NONE', #7186, #1522 ) ;
#9114 = CARTESIAN_POINT ( 'NONE',  ( 14.46874999795161720, -4.861323657744410554, 0.5109457054261454800 ) ) ;
#9115 = CYLINDRICAL_SURFACE ( 'NONE', #18225, 1.000000000000004441 ) ;
#9116 = CARTESIAN_POINT ( 'NONE',  ( 14.84374999795161543, 2.873153789725825913, 3.954556930911861112 ) ) ;
#9117 = EDGE_CURVE ( 'NONE', #13431, #13685, #6773, .T. ) ;
#9118 = DIRECTION ( 'NONE',  ( -1.000000000000000000, -0.000000000000000000, -0.000000000000000000 ) ) ;
#9119 = CARTESIAN_POINT ( 'NONE',  ( -9.580134541264520465, -14.56230589874905235, -32.00000000000000000 ) ) ;
#9120 = EDGE_LOOP ( 'NONE', ( #16837, #17978, #18380, #17729 ) ) ;
#9121 = CARTESIAN_POINT ( 'NONE',  ( -1.280903732194487166, -4.780397808154247308, -9.343749997951615427 ) ) ;
#9122 = CARTESIAN_POINT ( 'NONE',  ( 2.765633920072235963, 21.30679549418649543, -12.59161484032888723 ) ) ;
#9123 = VECTOR ( 'NONE', #16381, 1000.000000000000000 ) ;
#9124 = VERTEX_POINT ( 'NONE', #4467 ) ;
#9125 = CIRCLE ( 'NONE', #2998, 1.000000000000002665 ) ;
#9126 = CARTESIAN_POINT ( 'NONE',  ( 2.873153789725825025, 3.954556930911862000, -13.84374999795161543 ) ) ;
#9127 = DIRECTION ( 'NONE',  ( 0.000000000000000000, 0.8090169943749527803, -0.5877852522924655876 ) ) ;
#9128 = MANIFOLD_SOLID_BREP ( 'Extrude-Thin1', #11952 ) ;
#9129 = ORIENTED_EDGE ( 'NONE', *, *, #14437, .F. ) ;
#9130 = CARTESIAN_POINT ( 'NONE',  ( 7.812499995903224637, 5.387740456496233676, -2.068159791354184041 ) ) ;
#9131 = FACE_OUTER_BOUND ( 'NONE', #7532, .T. ) ;
#9132 = ORIENTED_EDGE ( 'NONE', *, *, #5781, .F. ) ;
#9133 = DIRECTION ( 'NONE',  ( -1.000000000000000000, -0.000000000000000000, 0.000000000000000000 ) ) ;
#9134 = ORIENTED_EDGE ( 'NONE', *, *, #11621, .T. ) ;
#9135 = CARTESIAN_POINT ( 'NONE',  ( -6.636868745521697477, -5.333637566582153156, -0.3148715423363437904 ) ) ;
#9136 = CIRCLE ( 'NONE', #14887, 1.000000000000000888 ) ;
#9137 = VERTEX_POINT ( 'NONE', #18864 ) ;
#9138 = B_SPLINE_CURVE_WITH_KNOTS ( 'NONE', 3,
 ( #4161, #10276, #15370, #13667 ),
 .UNSPECIFIED., .F., .F.,
 ( 4, 4 ),
 ( 0.005258139959819246867, 0.005948405594583413246 ),
 .UNSPECIFIED. ) ;
#9139 = DIRECTION ( 'NONE',  ( -0.5000000000000004441, 0.8660254037844383745, 0.000000000000000000 ) ) ;
#9140 = CIRCLE ( 'NONE', #16481, 28.06981291497571007 ) ;
#9141 = CARTESIAN_POINT ( 'NONE',  ( 2.000000000000000000, -2.000000000000002665, 41.99999999999999289 ) ) ;
#9142 = DIRECTION ( 'NONE',  ( -0.4330127018922180770, 0.7500000000000021094, 0.4999999999999979461 ) ) ;
#9143 = CYLINDRICAL_SURFACE ( 'NONE', #9455, 5.700000000000001954 ) ;
#9144 = CARTESIAN_POINT ( 'NONE',  ( 0.02436607992775934733, -2.336989772644440855, 24.63872515616082026 ) ) ;
#9145 = ORIENTED_EDGE ( 'NONE', *, *, #10548, .T. ) ;
#9146 = CARTESIAN_POINT ( 'NONE',  ( 2.783069004973548921, -5.408431875071614492, 23.92277630352793238 ) ) ;
#9147 = EDGE_CURVE ( 'NONE', #5524, #10504, #6914, .T. ) ;
#9148 =( NAMED_UNIT ( * ) PLANE_ANGLE_UNIT ( ) SI_UNIT ( $, .RADIAN. ) );
#9149 = AXIS2_PLACEMENT_3D ( 'NONE', #4621, #12627, #14024 ) ;
#9150 = ORIENTED_EDGE ( 'NONE', *, *, #14020, .F. ) ;
#9151 = AXIS2_PLACEMENT_3D ( 'NONE', #17928, #17731, #7295 ) ;
#9152 = CARTESIAN_POINT ( 'NONE',  ( 13.00000000000000000, 3.840809689103004576, -4.211671987713725862 ) ) ;
#9153 = CARTESIAN_POINT ( 'NONE',  ( -41.99999999999999289, -2.000000000000001776, -5.000000000000000000 ) ) ;
#9154 = ORIENTED_EDGE ( 'NONE', *, *, #10260, .F. ) ;
#9155 = CARTESIAN_POINT ( 'NONE',  ( 2.790000000000000036, 0.000000000000000000, 0.000000000000000000 ) ) ;
#9156 = CARTESIAN_POINT ( 'NONE',  ( 1.960886852992497653, -24.44424927289185590, 12.96989951879399072 ) ) ;
#9157 = CARTESIAN_POINT ( 'NONE',  ( -4.936344801571268093, 2.850000000000057820, -12.31249999590322552 ) ) ;
#9158 = ORIENTED_EDGE ( 'NONE', *, *, #9282, .F. ) ;
#9159 = CARTESIAN_POINT ( 'NONE',  ( 0.000000000000000000, 0.000000000000000000, -6.000000000000005329 ) ) ;
#9160 = ORIENTED_EDGE ( 'NONE', *, *, #7008, .F. ) ;
#9161 = CARTESIAN_POINT ( 'NONE',  ( 4.465502636338025688, -1.988169868018592856, -14.46874999795161720 ) ) ;
#9162 = FACE_OUTER_BOUND ( 'NONE', #14067, .T. ) ;
#9163 = VERTEX_POINT ( 'NONE', #1953 ) ;
#9164 = EDGE_CURVE ( 'NONE', #2645, #4579, #4246, .T. ) ;
#9165 = EDGE_LOOP ( 'NONE', ( #17062, #2340, #6589, #8258 ) ) ;
#9166 = CARTESIAN_POINT ( 'NONE',  ( 0.000000000000000000, 0.000000000000000000, -25.03750572909317285 ) ) ;
#9167 = AXIS2_PLACEMENT_3D ( 'NONE', #2283, #11492, #499 ) ;
#9168 = CARTESIAN_POINT ( 'NONE',  ( 1.988169868018593300, 4.465502636338024800, -9.843749997951615427 ) ) ;
#9169 = AXIS2_PLACEMENT_3D ( 'NONE', #18009, #4485, #18202 ) ;
#9170 = ORIENTED_EDGE ( 'NONE', *, *, #17494, .F. ) ;
#9171 = CARTESIAN_POINT ( 'NONE',  ( -12.32184790671639085, 13.12143529358541549, 32.00000000000000000 ) ) ;
#9172 = VERTEX_POINT ( 'NONE', #3758 ) ;
#9173 = EDGE_CURVE ( 'NONE', #1730, #6039, #8158, .T. ) ;
#9174 = DIRECTION ( 'NONE',  ( -1.000000000000000000, -0.000000000000000000, -0.000000000000000000 ) ) ;
#9175 = ORIENTED_EDGE ( 'NONE', *, *, #11867, .F. ) ;
#9176 = AXIS2_PLACEMENT_3D ( 'NONE', #8737, #1033, #15778 ) ;
#9177 = AXIS2_PLACEMENT_3D ( 'NONE', #431, #3429, #16946 ) ;
#9178 = DIRECTION ( 'NONE',  ( 1.224646799147353207E-16, -1.000000000000000000, 0.000000000000000000 ) ) ;
#9179 = CARTESIAN_POINT ( 'NONE',  ( 13.00000000000000000, -0.2705398332808414130, -4.881009025374877908 ) ) ;
#9180 = CARTESIAN_POINT ( 'NONE',  ( -36.00000000000000000, -6.000000000000000888, 7.347880794884120722E-16 ) ) ;
#9181 = EDGE_LOOP ( 'NONE', ( #12320, #8572, #7069, #3183 ) ) ;
#9182 = EDGE_LOOP ( 'NONE', ( #860, #9283, #2421, #14678 ) ) ;
#9183 = CARTESIAN_POINT ( 'NONE',  ( -2.000000000000000000, -5.000000000000001776, 37.99999999999999289 ) ) ;
#9184 =( NAMED_UNIT ( * ) PLANE_ANGLE_UNIT ( ) SI_UNIT ( $, .RADIAN. ) );
#9185 = FACE_OUTER_BOUND ( 'NONE', #14557, .T. ) ;
#9186 = VERTEX_POINT ( 'NONE', #7950 ) ;
#9187 = ADVANCED_FACE ( 'NONE', ( #466, #11168 ), #15967, .F. ) ;
#9188 = CARTESIAN_POINT ( 'NONE',  ( -36.00000000000000000, -2.000000000000000888, 2.000000000000000000 ) ) ;
#9189 = FACE_OUTER_BOUND ( 'NONE', #4064, .T. ) ;
#9190 = CARTESIAN_POINT ( 'NONE',  ( 0.7592463941534255412, -27.31305418910211813, 3.797885586973120287 ) ) ;
#9191 = FACE_OUTER_BOUND ( 'NONE', #18260, .T. ) ;
#9192 = EDGE_CURVE ( 'NONE', #8014, #6715, #19119, .T. ) ;
#9193 = AXIS2_PLACEMENT_3D ( 'NONE', #1917, #8013, #14127 ) ;
#9194 = CARTESIAN_POINT ( 'NONE',  ( 16.11901729331276556, 5.562305898749055011, 32.00000000000000000 ) ) ;
#9195 = VECTOR ( 'NONE', #14103, 1000.000000000000000 ) ;
#9196 = ORIENTED_EDGE ( 'NONE', *, *, #5425, .F. ) ;
#9197 = DIRECTION ( 'NONE',  ( 1.000000000000000000, -0.000000000000000000, -0.000000000000000000 ) ) ;
#9198 = EDGE_CURVE ( 'NONE', #17288, #14054, #16375, .T. ) ;
#9199 = FACE_OUTER_BOUND ( 'NONE', #5449, .T. ) ;
#9200 = MANIFOLD_SOLID_BREP ( 'Cut-Extrude1', #18617 ) ;
#9201 = ORIENTED_EDGE ( 'NONE', *, *, #1500, .F. ) ;
#9202 = DIRECTION ( 'NONE',  ( -0.000000000000000000, 0.000000000000000000, 1.000000000000000000 ) ) ;
#9203 = CARTESIAN_POINT ( 'NONE',  ( 7.078124996927420476, 4.584782303107579615, 2.647025296875021638 ) ) ;
#9204 = CARTESIAN_POINT ( 'NONE',  ( 91.50000000000000000, 4.898587196589412829E-16, -4.000000000000000000 ) ) ;
#9205 = DIRECTION ( 'NONE',  ( 0.000000000000000000, 0.000000000000000000, 1.000000000000000000 ) ) ;
#9206 = ADVANCED_FACE ( 'NONE', ( #2537 ), #9765, .T. ) ;
#9207 = VERTEX_POINT ( 'NONE', #7320 ) ;
#9208 = AXIS2_PLACEMENT_3D ( 'NONE', #5673, #17793, #16295 ) ;
#9209 = DIRECTION ( 'NONE',  ( 0.000000000000000000, 0.000000000000000000, 1.000000000000000000 ) ) ;
#9210 = CARTESIAN_POINT ( 'NONE',  ( 2.695436003842704764, -4.150607464521811174, -13.34374999795161365 ) ) ;
#9211 = CIRCLE ( 'NONE', #4733, 1.000000000000000888 ) ;
#9212 = EDGE_LOOP ( 'NONE', ( #7961, #15977, #3369, #10141 ) ) ;
#9213 = CARTESIAN_POINT ( 'NONE',  ( -1.001543065824775120E-15, -9.165435523385328409, -6.527800000000000047 ) ) ;
#9214 = LINE ( 'NONE', #3196, #15447 ) ;
#9215 = EDGE_CURVE ( 'NONE', #3690, #15613, #14950, .T. ) ;
#9216 = CARTESIAN_POINT ( 'NONE',  ( 8.500000000000007105, 5.574407415329156734, 1.493657965219523875 ) ) ;
#9217 = CYLINDRICAL_SURFACE ( 'NONE', #1512, 28.06981291497571362 ) ;
#9218 = VERTEX_POINT ( 'NONE', #13061 ) ;
#9219 = DIRECTION ( 'NONE',  ( 0.000000000000000000, 0.000000000000000000, 1.000000000000000000 ) ) ;
#9220 = CARTESIAN_POINT ( 'NONE',  ( 2.789999999999999147, 5.535312321043049266, -23.48180575137724446 ) ) ;
#9221 = ORIENTED_EDGE ( 'NONE', *, *, #13135, .F. ) ;
#9222 = CARTESIAN_POINT ( 'NONE',  ( 10.46874999795161720, -4.648860486681964055, 1.510506337161829027 ) ) ;
#9223 = CARTESIAN_POINT ( 'NONE',  ( 0.000000000000000000, -20.70663861606260170, -15.04425356660783031 ) ) ;
#9224 = CIRCLE ( 'NONE', #9541, 0.9999999999999974465 ) ;
#9225 = EDGE_LOOP ( 'NONE', ( #16785, #3609, #15227, #19185 ) ) ;
#9226 = EDGE_CURVE ( 'NONE', #5242, #13431, #19443, .T. ) ;
#9227 = ADVANCED_FACE ( 'NONE', ( #13440, #13156 ), #19344, .F. ) ;
#9228 = CARTESIAN_POINT ( 'NONE',  ( 2.500000000000002220, 0.000000000000000000, -8.800000000000023803 ) ) ;
#9229 = CARTESIAN_POINT ( 'NONE',  ( 0.000000000000000000, 0.000000000000000000, 0.000000000000000000 ) ) ;
#9230 = VERTEX_POINT ( 'NONE', #5729 ) ;
#9231 = FACE_OUTER_BOUND ( 'NONE', #14442, .T. ) ;
#9232 = DIRECTION ( 'NONE',  ( 0.8660254037844417052, -0.4999999999999947820, 0.000000000000000000 ) ) ;
#9233 = ORIENTED_EDGE ( 'NONE', *, *, #12851, .T. ) ;
#9234 = CARTESIAN_POINT ( 'NONE',  ( 13.00000000000000178, 7.960204194457801393E-16, -6.500000000000002665 ) ) ;
#9235 = EDGE_LOOP ( 'NONE', ( #4697, #2650, #7301, #3932 ) ) ;
#9237 = DIRECTION ( 'NONE',  ( -1.000000000000000000, -0.000000000000000000, -0.000000000000000000 ) ) ;
#9236 = AXIS2_PLACEMENT_3D ( 'NONE', #4435, #27, #1999 ) ;
#9238 = ORIENTED_EDGE ( 'NONE', *, *, #11112, .T. ) ;
#9239 = CARTESIAN_POINT ( 'NONE',  ( 2.790000000000076419, 2.133839912091138213, -24.22524813288759660 ) ) ;
#9240 = CARTESIAN_POINT ( 'NONE',  ( 0.000000000000000000, 0.000000000000000000, -35.00000000000000000 ) ) ;
#9241 = CARTESIAN_POINT ( 'NONE',  ( -5.700000000000001066, 1.090170143537592985E-15, -9.332722423957234170 ) ) ;
#9242 = CARTESIAN_POINT ( 'NONE',  ( 2.789999999999999147, -21.30679549418621832, -12.59161484032935618 ) ) ;
#9243 = VERTEX_POINT ( 'NONE', #2439 ) ;
#9244 = DIRECTION ( 'NONE',  ( 0.000000000000000000, 0.000000000000000000, 1.000000000000000000 ) ) ;
#9245 = CARTESIAN_POINT ( 'NONE',  ( -4.366025403784388637, -7.562177826491097044, 37.99999999999999289 ) ) ;
#9246 = VECTOR ( 'NONE', #17410, 1000.000000000000000 ) ;
#9247 = VERTEX_POINT ( 'NONE', #17663 ) ;
#9248 = ADVANCED_FACE ( 'NONE', ( #14664 ), #17956, .F. ) ;
#9249 = CARTESIAN_POINT ( 'NONE',  ( -4.762500000000000178, 5.832380380939270108E-16, -25.03750572909317285 ) ) ;
#9250 = CARTESIAN_POINT ( 'NONE',  ( 0.000000000000000000, 7.909232158575156824, -24.34211360614291664 ) ) ;
#9251 = ORIENTED_EDGE ( 'NONE', *, *, #8365, .T. ) ;
#9253 = LINE ( 'NONE', #7836, #11167 ) ;
#9252 = AXIS2_PLACEMENT_3D ( 'NONE', #18171, #13453, #19554 ) ;
#9254 = DIRECTION ( 'NONE',  ( 0.000000000000000000, 0.000000000000000000, -1.000000000000000000 ) ) ;
#9255 = EDGE_LOOP ( 'NONE', ( #19716, #8271, #10325, #4058, #5899 ) ) ;
#9256 = B_SPLINE_CURVE_WITH_KNOTS ( 'NONE', 3,
 ( #11008, #9419, #6291, #7996 ),
 .UNSPECIFIED., .F., .F.,
 ( 4, 4 ),
 ( 1.981826382900813409E-07, 0.0006887856082032219702 ),
 .UNSPECIFIED. ) ;
#9257 = CARTESIAN_POINT ( 'NONE',  ( -5.700000000000001066, 1.090170143537592985E-15, -10.64522241986045259 ) ) ;
#9258 = ORIENTED_EDGE ( 'NONE', *, *, #9370, .F. ) ;
#9259 = CARTESIAN_POINT ( 'NONE',  ( 0.006974657972265168107, -5.408388659524262287, 23.92335783895635970 ) ) ;
#9260 = VERTEX_POINT ( 'NONE', #4247 ) ;
#9261 = APPLICATION_PROTOCOL_DEFINITION ( 'draft international standard', 'automotive_design', 1998, #13526 ) ;
#9262 = DIRECTION ( 'NONE',  ( 0.000000000000000000, 0.000000000000000000, 1.000000000000000000 ) ) ;
#9263 = EDGE_CURVE ( 'NONE', #18451, #201, #19643, .T. ) ;
#9264 = VERTEX_POINT ( 'NONE', #952 ) ;
#9265 = EDGE_LOOP ( 'NONE', ( #5775, #10136, #4830, #19291 ) ) ;
#9266 = CARTESIAN_POINT ( 'NONE',  ( 6.626241948324199882, -16.73597674598852691, -35.00000000000000000 ) ) ;
#9267 = CARTESIAN_POINT ( 'NONE',  ( 8.843749997951615427, 2.873153789725825469, -3.954556930911862000 ) ) ;
#9268 = ORIENTED_EDGE ( 'NONE', *, *, #10994, .F. ) ;
#9269 = AXIS2_PLACEMENT_3D ( 'NONE', #15139, #10351, #1628 ) ;
#9270 = EDGE_CURVE ( 'NONE', #7513, #1540, #15819, .T. ) ;
#9271 = DIRECTION ( 'NONE',  ( -1.000000000000000000, -0.000000000000000000, -0.000000000000000000 ) ) ;
#9272 = VERTEX_POINT ( 'NONE', #11651 ) ;
#9273 = LINE ( 'NONE', #3857, #5820 ) ;
#9274 = DIRECTION ( 'NONE',  ( -1.000000000000000000, -0.000000000000000000, -0.000000000000000000 ) ) ;
#9275 = CARTESIAN_POINT ( 'NONE',  ( 0.006974693931641778172, 18.43727551351055283, -16.17543236987968669 ) ) ;
#9276 = VERTEX_POINT ( 'NONE', #10359 ) ;
#9277 = CIRCLE ( 'NONE', #18236, 4.000000000000000000 ) ;
#9278 = ORIENTED_EDGE ( 'NONE', *, *, #3959, .T. ) ;
#9279 = DIRECTION ( 'NONE',  ( -1.000000000000000000, -0.000000000000000000, -0.000000000000000000 ) ) ;
#9280 = AXIS2_PLACEMENT_3D ( 'NONE', #15800, #2382, #505 ) ;
#9281 = FACE_OUTER_BOUND ( 'NONE', #2273, .T. ) ;
#9282 = EDGE_CURVE ( 'NONE', #10204, #17548, #2147, .T. ) ;
#9283 = ORIENTED_EDGE ( 'NONE', *, *, #9892, .T. ) ;
#9284 = ORIENTED_EDGE ( 'NONE', *, *, #4503, .F. ) ;
#9285 = DIRECTION ( 'NONE',  ( -0.000000000000000000, -0.000000000000000000, -1.000000000000000000 ) ) ;
#9286 = DIRECTION ( 'NONE',  ( 0.000000000000000000, 0.000000000000000000, 1.000000000000000000 ) ) ;
#9287 = CARTESIAN_POINT ( 'NONE',  ( -3.255998204157480203, -17.85806462366060288, -35.00000000000000000 ) ) ;
#9288 = FACE_OUTER_BOUND ( 'NONE', #4532, .T. ) ;
#9289 = CARTESIAN_POINT ( 'NONE',  ( -3.499494075959816541, 3.499494075959816541, -8.968749997951611874 ) ) ;
#9290 = ORIENTED_EDGE ( 'NONE', *, *, #4073, .F. ) ;
#9291 = CARTESIAN_POINT ( 'NONE',  ( 1.749999999999998002, -27.68468304288255766, -4.633866840649213614 ) ) ;
#9292 = DIRECTION ( 'NONE',  ( 1.000000000000000000, 0.000000000000000000, 0.000000000000000000 ) ) ;
#9293 = TOROIDAL_SURFACE ( 'NONE', #6091, 24.12539914357697768, 8.000000000000000000 ) ;
#9294 = ORIENTED_EDGE ( 'NONE', *, *, #7675, .T. ) ;
#9295 = CARTESIAN_POINT ( 'NONE',  ( 7.500000000000005329, -3.143139765844555900, -4.840010801796527318 ) ) ;
#9296 = EDGE_CURVE ( 'NONE', #7908, #8102, #4344, .T. ) ;
#9297 = EDGE_CURVE ( 'NONE', #8927, #11311, #8146, .T. ) ;
#9298 = CARTESIAN_POINT ( 'NONE',  ( 7.937500000000001776, 1.560264056424248258, -0.06840592591720123794 ) ) ;
#9299 = PLANE ( 'NONE',  #15737 ) ;
#9300 = LINE ( 'NONE', #195, #1720 ) ;
#9301 = EDGE_CURVE ( 'NONE', #16271, #16569, #10074, .T. ) ;
#9302 = ORIENTED_EDGE ( 'NONE', *, *, #6565, .T. ) ;
#9303 = CYLINDRICAL_SURFACE ( 'NONE', #6273, 13.19999999999999929 ) ;
#9304 = SHAPE_REPRESENTATION_RELATIONSHIP ( 'NONE' , 'NONE' ,  #451, #2068 ) ;
#9305 = DIRECTION ( 'NONE',  ( 1.000000000000000000, -0.000000000000000000, -0.000000000000000000 ) ) ;
#9306 = SURFACE_SIDE_STYLE ('',( #297 ) ) ;
#9307 = ORIENTED_EDGE ( 'NONE', *, *, #4170, .F. ) ;
#9308 = CARTESIAN_POINT ( 'NONE',  ( 7.671566133830872047, 15.77352024078954784, -32.00000000000000000 ) ) ;
#9309 = AXIS2_PLACEMENT_3D ( 'NONE', #17395, #16461, #19350 ) ;
#9310 = DIRECTION ( 'NONE',  ( 0.000000000000000000, -1.374038396813314756E-15, -1.000000000000000000 ) ) ;
#9311 = DIRECTION ( 'NONE',  ( -1.000000000000000000, 0.000000000000000000, -0.000000000000000000 ) ) ;
#9312 = VECTOR ( 'NONE', #19242, 1000.000000000000000 ) ;
#9313 = CARTESIAN_POINT ( 'NONE',  ( 1.255998204157470211, -17.85806462366060288, -32.00000000000000000 ) ) ;
#9314 = ORIENTED_EDGE ( 'NONE', *, *, #7334, .F. ) ;
#9315 = DIRECTION ( 'NONE',  ( -1.000000000000000000, -0.000000000000000000, -0.000000000000000000 ) ) ;
#9316 = CARTESIAN_POINT ( 'NONE',  ( -0.000000000000000000, 0.000000000000000000, 0.000000000000000000 ) ) ;
#9317 = ORIENTED_EDGE ( 'NONE', *, *, #9460, .T. ) ;
#9318 = CARTESIAN_POINT ( 'NONE',  ( 11.34374999795161543, -4.888101187500005551, 0.7741991708318548548 ) ) ;
#9319 = CARTESIAN_POINT ( 'NONE',  ( -5.476417968967388639, 17.43449690031536292, -32.00000000000000000 ) ) ;
#9320 = VERTEX_POINT ( 'NONE', #11751 ) ;
#9321 = ITEM_DEFINED_TRANSFORMATION ( 'NONE', 'NONE', #14355,  #16724 ) ;
#9322 = AXIS2_PLACEMENT_3D ( 'NONE', #17319, #17125, #4816 ) ;
#9323 = VECTOR ( 'NONE', #10305, 1000.000000000000000 ) ;
#9324 = CARTESIAN_POINT ( 'NONE',  ( 0.7741991708318884946, 4.888101187500000222, -11.96874999795161365 ) ) ;
#9325 = CARTESIAN_POINT ( 'NONE',  ( 2.789999999999999147, 15.04425356660790136, -18.18163861606255338 ) ) ;
#9326 = EDGE_LOOP ( 'NONE', ( #5680, #953, #983, #1757 ) ) ;
#9327 = FACE_BOUND ( 'NONE', #18704, .T. ) ;
#9328 = LINE ( 'NONE', #12135, #10362 ) ;
#9329 = EDGE_CURVE ( 'NONE', #17360, #569, #1188, .T. ) ;
#9330 = VERTEX_POINT ( 'NONE', #15148 ) ;
#9331 = CARTESIAN_POINT ( 'NONE',  ( 0.000000000000000000, -18.28042085475266632, -15.74360496233403239 ) ) ;
#9332 = ORIENTED_EDGE ( 'NONE', *, *, #5459, .T. ) ;
#9333 = ADVANCED_FACE ( 'NONE', ( #19648 ), #1444, .T. ) ;
#9334 = LINE ( 'NONE', #13834, #14945 ) ;
#9335 = ORIENTED_EDGE ( 'NONE', *, *, #13822, .T. ) ;
#9336 = B_SPLINE_CURVE_WITH_KNOTS ( 'NONE', 1,
 ( #15844, #12647 ),
 .UNSPECIFIED., .F., .F.,
 ( 2, 2 ),
 ( 0.000000000000000000, 1.000000000000000000 ),
 .UNSPECIFIED. ) ;
#9337 = CARTESIAN_POINT ( 'NONE',  ( 2.789999999999999147, 0.000000000000000000, 0.000000000000000000 ) ) ;
#9338 = CARTESIAN_POINT ( 'NONE',  ( -1.255998204157475318, -17.85806462366060288, 35.00000000000000000 ) ) ;
#9339 = DIRECTION ( 'NONE',  ( 0.000000000000000000, 0.000000000000000000, 1.000000000000000000 ) ) ;
#9340 = VECTOR ( 'NONE', #4081, 1000.000000000000000 ) ;
#9341 = CARTESIAN_POINT ( 'NONE',  ( 0.8291131470075423504, 24.44424927289185945, 12.96989951879416125 ) ) ;
#9342 = EDGE_CURVE ( 'NONE', #18696, #8532, #1636, .T. ) ;
#9343 = VERTEX_POINT ( 'NONE', #7631 ) ;
#9344 = VECTOR ( 'NONE', #1606, 1000.000000000000000 ) ;
#9345 = DIRECTION ( 'NONE',  ( -1.000000000000000000, -6.419766481290786633E-33, 0.000000000000000000 ) ) ;
#9346 =( LENGTH_UNIT ( ) NAMED_UNIT ( * ) SI_UNIT ( .MILLI., .METRE. ) );
#9347 = CONICAL_SURFACE ( 'NONE', #4537, 3.889375000000000693, 0.9599310885968779239 ) ;
#9348 = DIRECTION ( 'NONE',  ( -0.4999999999999980016, -0.7500000000000048850, 0.4330127018922129700 ) ) ;
#9349 = ADVANCED_FACE ( 'NONE', ( #8947 ), #5930, .F. ) ;
#9350 = CARTESIAN_POINT ( 'NONE',  ( 11.58013454126452579, -14.56230589874905412, -32.00000000000000000 ) ) ;
#9351 = DIRECTION ( 'NONE',  ( -0.000000000000000000, 1.000000000000000000, 1.224646799147353207E-16 ) ) ;
#9352 = ORIENTED_EDGE ( 'NONE', *, *, #744, .T. ) ;
#9353 = VECTOR ( 'NONE', #8056, 1000.000000000000000 ) ;
#9354 = AXIS2_PLACEMENT_3D ( 'NONE', #17072, #16783, #19672 ) ;
#9355 = CARTESIAN_POINT ( 'NONE',  ( -34.92499999999994742, 0.000000000000000000, 0.000000000000000000 ) ) ;
#9356 = AXIS2_PLACEMENT_3D ( 'NONE', #6484, #2293, #11109 ) ;
#9357 = VERTEX_POINT ( 'NONE', #13845 ) ;
#9358 = CARTESIAN_POINT ( 'NONE',  ( -15.87499999999998579, -1.734723475976807094E-15, 0.000000000000000000 ) ) ;
#9359 = VERTEX_POINT ( 'NONE', #10454 ) ;
#9360 = SHAPE_DEFINITION_REPRESENTATION ( #6640, #2588 ) ;
#9361 = DIRECTION ( 'NONE',  ( -0.3826834323650905034, -0.9238795325112865164, 0.000000000000000000 ) ) ;
#9362 = CARTESIAN_POINT ( 'NONE',  ( 8.343749997951611874, 4.942249507334556924, -0.2590123213420971182 ) ) ;
#9363 = AXIS2_PLACEMENT_3D ( 'NONE', #11762, #3048, #19754 ) ;
#9364 = ORIENTED_EDGE ( 'NONE', *, *, #10069, .T. ) ;
#9365 = ORIENTED_EDGE ( 'NONE', *, *, #15682, .T. ) ;
#9366 = CARTESIAN_POINT ( 'NONE',  ( 91.50000000000000000, 4.898587196589412829E-16, 4.000000000000000000 ) ) ;
#9367 =( REPRESENTATION_RELATIONSHIP ('NONE','NONE', #18211, #4652 ) REPRESENTATION_RELATIONSHIP_WITH_TRANSFORMATION ( #3314 )SHAPE_REPRESENTATION_RELATIONSHIP( ) );
#9368 = CARTESIAN_POINT ( 'NONE',  ( 6.843749997951615427, 0.000000000000000000, -4.888101187500000222 ) ) ;
#9369 = VERTEX_POINT ( 'NONE', #1340 ) ;
#9370 = EDGE_CURVE ( 'NONE', #2028, #5529, #12941, .T. ) ;
#9371 = COLOUR_RGB ( '', 0.72549020, 0.75294118, 0.79215686) ;
#9372 = CARTESIAN_POINT ( 'NONE',  ( 0.000000000000000000, 15.04425356660790136, -18.18163861606255338 ) ) ;
#9373 = ADVANCED_FACE ( 'NONE', ( #7421 ), #13546, .T. ) ;
#9374 = ORIENTED_EDGE ( 'NONE', *, *, #174, .F. ) ;
#9375 = CIRCLE ( 'NONE', #8071, 1.000000000000000888 ) ;
#9376 = AXIS2_PLACEMENT_3D ( 'NONE', #19336, #5626, #10613 ) ;
#9377 = CARTESIAN_POINT ( 'NONE',  ( 12.96874999795161543, -0.2590123213420631454, -4.942249507334558700 ) ) ;
#9378 = CARTESIAN_POINT ( 'NONE',  ( 4.200000000000001954, 0.000000000000000000, -6.000000000000005329 ) ) ;
#9379 = CARTESIAN_POINT ( 'NONE',  ( 13.00000000000000178, -0.4594918047638649194, -4.866883308198429958 ) ) ;
#9380 = FACE_BOUND ( 'NONE', #7145, .T. ) ;
#9381 = ORIENTED_EDGE ( 'NONE', *, *, #11018, .F. ) ;
#9382 = EDGE_CURVE ( 'NONE', #18748, #15548, #800, .T. ) ;
#9383 = CARTESIAN_POINT ( 'NONE',  ( -2.000000000000001776, 0.000000000000000000, 4.400000000000000355 ) ) ;
#9384 = CARTESIAN_POINT ( 'NONE',  ( 1.749999999999998002, -20.02152543075331081, -19.67366047555553266 ) ) ;
#9385 = ORIENTED_EDGE ( 'NONE', *, *, #12390, .F. ) ;
#9386 = VERTEX_POINT ( 'NONE', #10547 ) ;
#9387 = CARTESIAN_POINT ( 'NONE',  ( 2.789999999999999147, 12.52067188844381107, -20.62201879784899461 ) ) ;
#9388 = CARTESIAN_POINT ( 'NONE',  ( 6.929096493834647319, 2.870125742738179664, 12.00000000000000000 ) ) ;
#9389 = LINE ( 'NONE', #80, #5748 ) ;
#9390 = AXIS2_PLACEMENT_3D ( 'NONE', #10117, #10027, #6795 ) ;
#9391 = EDGE_CURVE ( 'NONE', #17967, #12806, #140, .T. ) ;
#9392 = CARTESIAN_POINT ( 'NONE',  ( -5.626241948324210540, -16.73597674598852336, 35.00000000000000000 ) ) ;
#9393 = CARTESIAN_POINT ( 'NONE',  ( -2.444050593750049849, -4.233219804643852946, -6.843749997951615427 ) ) ;
#9394 = EDGE_LOOP ( 'NONE', ( #19157, #6153, #13221, #7804 ) ) ;
#9395 = DIRECTION ( 'NONE',  ( 0.000000000000000000, 0.000000000000000000, 1.000000000000000000 ) ) ;
#9396 = CARTESIAN_POINT ( 'NONE',  ( 10.34374999795161543, -4.409619785863921670, 2.246813503491803310 ) ) ;
#9397 = MANIFOLD_SOLID_BREP ( 'EndChamfer', #19571 ) ;
#9398 = PRESENTATION_LAYER_ASSIGNMENT (  '', '', ( #8761 ) ) ;
#9399 = VERTEX_POINT ( 'NONE', #3137 ) ;
#9400 = CARTESIAN_POINT ( 'NONE',  ( 2.765633920072235075, 24.63872515616082737, -2.336989772644355590 ) ) ;
#9401 = EDGE_CURVE ( 'NONE', #17188, #5932, #6527, .T. ) ;
#9402 = DIRECTION ( 'NONE',  ( 1.000000000000000000, 0.000000000000000000, 0.000000000000000000 ) ) ;
#9403 = CIRCLE ( 'NONE', #5871, 8.073750000000021743 ) ;
#9404 = DIRECTION ( 'NONE',  ( -1.000000000000000000, -0.000000000000000000, -0.000000000000000000 ) ) ;
#9405 = DIRECTION ( 'NONE',  ( 1.000000000000000000, 0.000000000000000000, 0.000000000000000000 ) ) ;
#9406 = CARTESIAN_POINT ( 'NONE',  ( -0.9027913098498961952, -5.699999999999994849, -11.50000000000000355 ) ) ;
#9407 = ORIENTED_EDGE ( 'NONE', *, *, #8797, .T. ) ;
#9408 = CARTESIAN_POINT ( 'NONE',  ( 13.46874999795161543, 3.954556930911862000, 2.873153789725825025 ) ) ;
#9409 = DIRECTION ( 'NONE',  ( -1.000000000000000000, 0.000000000000000000, 0.000000000000000000 ) ) ;
#9410 = LINE ( 'NONE', #12313, #2255 ) ;
#9411 = ORIENTED_EDGE ( 'NONE', *, *, #17001, .F. ) ;
#9412 = LINE ( 'NONE', #103, #3113 ) ;
#9413 = AXIS2_PLACEMENT_3D ( 'NONE', #11051, #15363, #1648 ) ;
#9414 =( NAMED_UNIT ( * ) SI_UNIT ( $, .STERADIAN. ) SOLID_ANGLE_UNIT ( ) );
#9415 = CARTESIAN_POINT ( 'NONE',  ( 10.46874999795161720, 3.632567103900523620, 3.270778111535338262 ) ) ;
#9416 = DIRECTION ( 'NONE',  ( 0.000000000000000000, 0.000000000000000000, 1.000000000000000000 ) ) ;
#9417 = ADVANCED_FACE ( 'NONE', ( #18443 ), #10844, .F. ) ;
#9418 = ORIENTED_EDGE ( 'NONE', *, *, #11042, .F. ) ;
#9419 = CARTESIAN_POINT ( 'NONE',  ( 2.783025342027734439, -23.92335783895641299, 5.408388659523998498 ) ) ;
#9420 = CARTESIAN_POINT ( 'NONE',  ( 2.789679245949062913, -20.70663861606260525, -12.51925356660783528 ) ) ;
#9421 = VERTEX_POINT ( 'NONE', #12444 ) ;
#9422 = AXIS2_PLACEMENT_3D ( 'NONE', #17031, #5015, #5105 ) ;
#9423 = CARTESIAN_POINT ( 'NONE',  ( 8.000000000000005329, -2.318398865532001363, -5.207209108562852684 ) ) ;
#9424 = LINE ( 'NONE', #14111, #18091 ) ;
#9425 = ORIENTED_EDGE ( 'NONE', *, *, #11318, .T. ) ;
#9426 = EDGE_CURVE ( 'NONE', #6765, #13330, #4950, .T. ) ;
#9427 = CONTEXT_DEPENDENT_SHAPE_REPRESENTATION ( #2832, #17853 ) ;
#9428 = VECTOR ( 'NONE', #6985, 1000.000000000000000 ) ;
#9429 = CARTESIAN_POINT ( 'NONE',  ( -16.68117051311640253, -3.372863662543042818, -35.00000000000000000 ) ) ;
#9430 = DIRECTION ( 'NONE',  ( -1.000000000000000000, -0.000000000000000000, -0.000000000000000000 ) ) ;
#9431 = MANIFOLD_SOLID_BREP ( 'OuterRace', #5237 ) ;
#9432 = ORIENTED_EDGE ( 'NONE', *, *, #8960, .F. ) ;
#9433 = FACE_OUTER_BOUND ( 'NONE', #934, .T. ) ;
#9434 = DIRECTION ( 'NONE',  ( 0.000000000000000000, 1.000000000000000000, 0.000000000000000000 ) ) ;
#9435 = ORIENTED_EDGE ( 'NONE', *, *, #6844, .F. ) ;
#9436 = CARTESIAN_POINT ( 'NONE',  ( -7.626241948324210540, -16.73597674598852336, 35.00000000000000000 ) ) ;
#9437 = ORIENTED_EDGE ( 'NONE', *, *, #19437, .F. ) ;
#9438 = CARTESIAN_POINT ( 'NONE',  ( -36.00000000000000000, 1.999999999999999112, 5.000000000000000000 ) ) ;
#9439 = EDGE_LOOP ( 'NONE', ( #9547, #11152 ) ) ;
#9440 = DIRECTION ( 'NONE',  ( 1.000000000000000000, 0.000000000000000000, 0.000000000000000000 ) ) ;
#9441 = FACE_OUTER_BOUND ( 'NONE', #19138, .T. ) ;
#9442 = EDGE_CURVE ( 'NONE', #6035, #15913, #486, .T. ) ;
#9443 = CARTESIAN_POINT ( 'NONE',  ( -5.700000000000001066, -0.2987243419133009947, -9.165444847914514526 ) ) ;
#9444 = VECTOR ( 'NONE', #3184, 1000.000000000000000 ) ;
#9445 = CARTESIAN_POINT ( 'NONE',  ( -1.310841663519413114, 0.000000000000000000, 0.000000000000000000 ) ) ;
#9446 = ORIENTED_EDGE ( 'NONE', *, *, #1400, .F. ) ;
#9447 = LINE ( 'NONE', #16853, #8068 ) ;
#9448 = DIRECTION ( 'NONE',  ( 0.000000000000000000, 0.000000000000000000, -1.000000000000000000 ) ) ;
#9449 = EDGE_CURVE ( 'NONE', #720, #15404, #2385, .T. ) ;
#9450 = APPLICATION_CONTEXT ( 'automotive_design' ) ;
#9451 = ORIENTED_EDGE ( 'NONE', *, *, #276, .F. ) ;
#9452 = CARTESIAN_POINT ( 'NONE',  ( -1.310841663519413114, 0.000000000000000000, 0.000000000000000000 ) ) ;
#9453 = DIRECTION ( 'NONE',  ( -1.000000000000000000, 0.000000000000000000, 0.000000000000000000 ) ) ;
#9454 = VERTEX_POINT ( 'NONE', #11603 ) ;
#9455 = AXIS2_PLACEMENT_3D ( 'NONE', #15248, #1630, #10936 ) ;
#9456 = CARTESIAN_POINT ( 'NONE',  ( 9.000000000000005329, -5.207209108562803834, -2.318398865532109721 ) ) ;
#9457 = LINE ( 'NONE', #7741, #19668 ) ;
#9458 = AXIS2_PLACEMENT_3D ( 'NONE', #6411, #12741, #11142 ) ;
#9459 = ORIENTED_EDGE ( 'NONE', *, *, #15318, .T. ) ;
#9460 = EDGE_CURVE ( 'NONE', #2982, #17056, #4762, .T. ) ;
#9461 = CYLINDRICAL_SURFACE ( 'NONE', #6202, 3.000000000000000000 ) ;
#9462 = ORIENTED_EDGE ( 'NONE', *, *, #14281, .F. ) ;
#9463 = PRODUCT_CONTEXT ( 'NONE', #1638, 'mechanical' ) ;
#9464 = CARTESIAN_POINT ( 'NONE',  ( 5.510910596163084625E-16, 18.00000000000000355, -35.00000000000000000 ) ) ;
#9465 = CARTESIAN_POINT ( 'NONE',  ( 7.968749997951616315, 4.942249507334556924, -0.2590123213420971182 ) ) ;
#9466 = ORIENTED_EDGE ( 'NONE', *, *, #11919, .F. ) ;
#9467 = VERTEX_POINT ( 'NONE', #12815 ) ;
#9468 = CARTESIAN_POINT ( 'NONE',  ( 0.07186815222488118771, 24.78765742476146272, -5.344160105508446001 ) ) ;
#9469 = B_SPLINE_CURVE_WITH_KNOTS ( 'NONE', 1,
 ( #5309, #10215 ),
 .UNSPECIFIED., .F., .F.,
 ( 2, 2 ),
 ( 0.000000000000000000, 1.000000000000000000 ),
 .UNSPECIFIED. ) ;
#9470 = FACE_OUTER_BOUND ( 'NONE', #9849, .T. ) ;
#9471 = EDGE_CURVE ( 'NONE', #12976, #4769, #5202, .T. ) ;
#9472 = ORIENTED_EDGE ( 'NONE', *, *, #14224, .T. ) ;
#9473 = CIRCLE ( 'NONE', #6564, 3.000000000000000000 ) ;
#9474 = AXIS2_PLACEMENT_3D ( 'NONE', #12421, #4911, #8106 ) ;
#9475 = DIRECTION ( 'NONE',  ( 0.000000000000000000, 0.000000000000000000, 1.000000000000000000 ) ) ;
#9476 = ORIENTED_EDGE ( 'NONE', *, *, #3198, .T. ) ;
#9477 = PLANE ( 'NONE',  #8600 ) ;
#9478 = CARTESIAN_POINT ( 'NONE',  ( 0.000000000000000000, -20.70663861606282197, 15.04425356660753188 ) ) ;
#9479 = FACE_BOUND ( 'NONE', #19756, .T. ) ;
#9480 = AXIS2_PLACEMENT_3D ( 'NONE', #2184, #6774, #3685 ) ;
#9481 = EDGE_LOOP ( 'NONE', ( #672, #18412 ) ) ;
#9482 = CARTESIAN_POINT ( 'NONE',  ( -3.476417968967383754, 17.43449690031536292, 32.00000000000000000 ) ) ;
#9483 =( NAMED_UNIT ( * ) SI_UNIT ( $, .STERADIAN. ) SOLID_ANGLE_UNIT ( ) );
#9484 = DIRECTION ( 'NONE',  ( -0.4999999999999979461, 0.000000000000000000, -0.8660254037844398178 ) ) ;
#9485 = VECTOR ( 'NONE', #17388, 1000.000000000000227 ) ;
#9486 = VERTEX_POINT ( 'NONE', #10112 ) ;
#9487 = ORIENTED_EDGE ( 'NONE', *, *, #2767, .F. ) ;
#9488 = DIRECTION ( 'NONE',  ( 0.000000000000000000, 0.000000000000000000, 1.000000000000000000 ) ) ;
#9489 = ADVANCED_BREP_SHAPE_REPRESENTATION ( '', ( #16364, #16724 ), #15776 ) ;
#9490 = CARTESIAN_POINT ( 'NONE',  ( 0.02436607992776325046, 16.37294372382858398, 18.55949924794898465 ) ) ;
#9491 = CARTESIAN_POINT ( 'NONE',  ( -1.899999999999999023, 0.000000000000000000, 0.000000000000000000 ) ) ;
#9492 = CARTESIAN_POINT ( 'NONE',  ( -41.99999999999999289, -2.000000000000001776, 2.000000000000000000 ) ) ;
#9493 = CARTESIAN_POINT ( 'NONE',  ( -4.936344801571268093, 2.850000000000057820, -12.31249999590322552 ) ) ;
#9494 = ORIENTED_EDGE ( 'NONE', *, *, #6590, .F. ) ;
#9495 = DIRECTION ( 'NONE',  ( 0.000000000000000000, 0.000000000000000000, -1.000000000000000000 ) ) ;
#9496 = CARTESIAN_POINT ( 'NONE',  ( 12.84374999795161543, -4.648860486681943627, -1.510506337161893642 ) ) ;
#9497 = VECTOR ( 'NONE', #1179, 1000.000000000000000 ) ;
#9498 = ORIENTED_EDGE ( 'NONE', *, *, #11932, .T. ) ;
#9499 = CARTESIAN_POINT ( 'NONE',  ( 12.96874999795161543, 4.150607464521828938, -2.695436003842674566 ) ) ;
#9500 = TOROIDAL_SURFACE ( 'NONE', #869, 6.200000000000020606, 0.2000000000000005107 ) ;
#9501 = FACE_OUTER_BOUND ( 'NONE', #17986, .T. ) ;
#9502 = CARTESIAN_POINT ( 'NONE',  ( 2.299999999999996270, 0.000000000000000000, 0.000000000000000000 ) ) ;
#9503 = CARTESIAN_POINT ( 'NONE',  ( -20.63749999999999574, 0.000000000000000000, 0.000000000000000000 ) ) ;
#9504 = CARTESIAN_POINT ( 'NONE',  ( 2.620002426024508502, -5.142044285764769462, -9.500000000000003553 ) ) ;
#9505 = VERTEX_POINT ( 'NONE', #11320 ) ;
#9506 = CARTESIAN_POINT ( 'NONE',  ( 1.749999999999998002, -24.89775460606842117, 12.96210679857777137 ) ) ;
#9507 =( LENGTH_UNIT ( ) NAMED_UNIT ( * ) SI_UNIT ( .MILLI., .METRE. ) );
#9508 = CARTESIAN_POINT ( 'NONE',  ( -3.954556930911881096, -2.873153789725797935, -14.46874999795161720 ) ) ;
#9509 = SURFACE_STYLE_USAGE ( .BOTH. , #9306 ) ;
#9510 = ORIENTED_EDGE ( 'NONE', *, *, #667, .F. ) ;
#9511 = DIRECTION ( 'NONE',  ( 1.000000000000000000, 0.000000000000000000, 0.000000000000000000 ) ) ;
#9512 = VECTOR ( 'NONE', #16135, 1000.000000000000000 ) ;
#9513 = CARTESIAN_POINT ( 'NONE',  ( -18.96448111170889206, 1.130229351527647585, -32.00000000000000000 ) ) ;
#9514 = ADVANCED_FACE ( 'NONE', ( #17421 ), #8307, .F. ) ;
#9515 = CIRCLE ( 'NONE', #6936, 5.700000000000002842 ) ;
#9516 = CARTESIAN_POINT ( 'NONE',  ( 15.19790265903627358, 9.644882309621939598, 32.00000000000000000 ) ) ;
#9517 = FACE_OUTER_BOUND ( 'NONE', #2206, .T. ) ;
#9518 = ORIENTED_EDGE ( 'NONE', *, *, #10121, .F. ) ;
#9519 = CARTESIAN_POINT ( 'NONE',  ( -4.200000000000001066, 5.143516556418885886E-16, 0.000000000000000000 ) ) ;
#9520 = CARTESIAN_POINT ( 'NONE',  ( 0.7741991708318884946, 4.888101187500000222, -12.34374999795161543 ) ) ;
#9521 = VERTEX_POINT ( 'NONE', #17050 ) ;
#9522 = DIRECTION ( 'NONE',  ( 0.000000000000000000, -3.552713678800500929E-15, 1.000000000000000000 ) ) ;
#9523 = DIRECTION ( 'NONE',  ( -1.000000000000000000, 0.000000000000000000, 0.000000000000000000 ) ) ;
#9524 = ORIENTED_EDGE ( 'NONE', *, *, #7599, .T. ) ;
#9525 = AXIS2_PLACEMENT_3D ( 'NONE', #16107, #19186, #3989 ) ;
#9526 = CIRCLE ( 'NONE', #7905, 0.9999999999999974465 ) ;
#9527 = CARTESIAN_POINT ( 'NONE',  ( 0.000000000000000000, -5.000000000000001776, 37.99999999999999289 ) ) ;
#9528 = CARTESIAN_POINT ( 'NONE',  ( 1.960886852992457241, 24.44424927289185945, 12.96989951879416125 ) ) ;
#9529 = ORIENTED_EDGE ( 'NONE', *, *, #12078, .F. ) ;
#9530 = FACE_OUTER_BOUND ( 'NONE', #4689, .T. ) ;
#9531 = DIRECTION ( 'NONE',  ( -0.4999999999999979461, 0.000000000000000000, 0.8660254037844398178 ) ) ;
#9532 = ORIENTED_EDGE ( 'NONE', *, *, #6990, .F. ) ;
#9533 = FACE_OUTER_BOUND ( 'NONE', #2454, .T. ) ;
#9534 = EDGE_LOOP ( 'NONE', ( #11041, #7820, #5111, #16230 ) ) ;
#9535 = CARTESIAN_POINT ( 'NONE',  ( 5.700000000000001954, 0.000000000000000000, 0.000000000000000000 ) ) ;
#9536 = ORIENTED_EDGE ( 'NONE', *, *, #4191, .T. ) ;
#9537 = CARTESIAN_POINT ( 'NONE',  ( 2.765633920072238183, -5.391175441198789109, 24.15498966839961170 ) ) ;
#9538 = EDGE_CURVE ( 'NONE', #3268, #3153, #15917, .T. ) ;
#9539 = FACE_OUTER_BOUND ( 'NONE', #1770, .T. ) ;
#9540 = CARTESIAN_POINT ( 'NONE',  ( -17.96448111170888851, 1.130229351527647585, 32.00000000000000000 ) ) ;
#9541 = AXIS2_PLACEMENT_3D ( 'NONE', #2749, #16574, #14968 ) ;
#9542 = CARTESIAN_POINT ( 'NONE',  ( 0.5109457054261454800, -4.861323657744410554, -14.84374999795161543 ) ) ;
#9543 = AXIS2_PLACEMENT_3D ( 'NONE', #15194, #13591, #1583 ) ;
#9544 = VERTEX_POINT ( 'NONE', #3803 ) ;
#9545 = CARTESIAN_POINT ( 'NONE',  ( -2.300000000000000711, 1.077689183249673564E-15, 8.800000000000022027 ) ) ;
#9546 = CARTESIAN_POINT ( 'NONE',  ( 2.789999999999999147, -20.70663861606260170, -12.51925356660783528 ) ) ;
#9547 = ORIENTED_EDGE ( 'NONE', *, *, #13135, .T. ) ;
#9548 = DIRECTION ( 'NONE',  ( 1.000000000000000000, 0.000000000000000000, 0.000000000000000000 ) ) ;
#9549 = CARTESIAN_POINT ( 'NONE',  ( 2.765633920072236407, 2.336989772644613161, -24.63872515616080250 ) ) ;
#9550 = ADVANCED_FACE ( 'NONE', ( #712 ), #4833, .F. ) ;
#9551 = CARTESIAN_POINT ( 'NONE',  ( 0.2590123213420630899, -4.942249507334558700, -7.968749997951616315 ) ) ;
#9552 = EDGE_CURVE ( 'NONE', #15782, #19176, #6887, .T. ) ;
#9553 = CIRCLE ( 'NONE', #11770, 4.000000000000000000 ) ;
#9554 = ORIENTED_EDGE ( 'NONE', *, *, #5882, .F. ) ;
#9555 = DIRECTION ( 'NONE',  ( 1.000000000000000000, 0.000000000000000000, 0.000000000000000000 ) ) ;
#9556 = CARTESIAN_POINT ( 'NONE',  ( 12.81249999590322552, 3.631840208645857437, -4.484949146646330931 ) ) ;
#9557 = ORIENTED_EDGE ( 'NONE', *, *, #1760, .F. ) ;
#9558 = EDGE_CURVE ( 'NONE', #14379, #12547, #14218, .T. ) ;
#9559 = VERTEX_POINT ( 'NONE', #8602 ) ;
#9560 = APPLICATION_PROTOCOL_DEFINITION ( 'draft international standard', 'automotive_design', 1998, #514 ) ;
#9561 = CARTESIAN_POINT ( 'NONE',  ( 0.000000000000000000, 23.48180575137739368, -5.535312321042471062 ) ) ;
#9562 = DIRECTION ( 'NONE',  ( -1.000000000000000000, 0.000000000000000000, 0.000000000000000000 ) ) ;
#9563 = EDGE_LOOP ( 'NONE', ( #1480, #14156, #13619, #7902 ) ) ;
#9564 = ORIENTED_EDGE ( 'NONE', *, *, #16891, .F. ) ;
#9565 = EDGE_CURVE ( 'NONE', #4459, #7726, #2396, .T. ) ;
#9566 = CARTESIAN_POINT ( 'NONE',  ( 6.634287453978997107, -5.335127875949193132, -0.3142460757452261721 ) ) ;
#9567 = DIRECTION ( 'NONE',  ( 0.000000000000000000, 0.000000000000000000, 1.000000000000000000 ) ) ;
#9568 = ORIENTED_EDGE ( 'NONE', *, *, #8145, .F. ) ;
#9569 = AXIS2_PLACEMENT_3D ( 'NONE', #4142, #13148, #4047 ) ;
#9570 = DIRECTION ( 'NONE',  ( 1.000000000000000000, 0.000000000000000000, 0.000000000000000000 ) ) ;
#9571 = ADVANCED_FACE ( 'NONE', ( #14710 ), #8212, .F. ) ;
#9572 = ORIENTED_EDGE ( 'NONE', *, *, #7851, .T. ) ;
#9573 = EDGE_CURVE ( 'NONE', #15108, #5313, #17904, .T. ) ;
#9574 = CARTESIAN_POINT ( 'NONE',  ( -4.936344801571327601, -2.849999999999954792, -11.00000000000000711 ) ) ;
#9575 = FACE_OUTER_BOUND ( 'NONE', #17898, .T. ) ;
#9576 = FACE_BOUND ( 'NONE', #17488, .T. ) ;
#9577 = ORIENTED_EDGE ( 'NONE', *, *, #7263, .F. ) ;
#9578 = CARTESIAN_POINT ( 'NONE',  ( -15.00000000000000355, 3.434748899119117294, -2.750000000000002220 ) ) ;
#9579 = FILL_AREA_STYLE ('',( #3371 ) ) ;
#9580 = ORIENTED_EDGE ( 'NONE', *, *, #5252, .T. ) ;
#9581 = VERTEX_POINT ( 'NONE', #19599 ) ;
#9582 = ADVANCED_FACE ( 'NONE', ( #1197 ), #17806, .T. ) ;
#9583 = CARTESIAN_POINT ( 'NONE',  ( 2.718184745196086549, -12.74223776959184207, -21.92234060054359901 ) ) ;
#9584 = AXIS2_PLACEMENT_3D ( 'NONE', #12068, #1359, #4657 ) ;
#9585 = DIRECTION ( 'NONE',  ( 0.000000000000000000, 0.000000000000000000, 1.000000000000000000 ) ) ;
#9586 = CARTESIAN_POINT ( 'NONE',  ( 1.510506337161861223, 4.648860486681953397, -12.46874999795161543 ) ) ;
#9587 = EDGE_LOOP ( 'NONE', ( #14902, #3308, #176, #1963 ) ) ;
#9588 = EDGE_CURVE ( 'NONE', #3997, #13012, #8159, .T. ) ;
#9589 = CARTESIAN_POINT ( 'NONE',  ( 13.46874999795161543, 4.465502636338051445, -1.988169868018530906 ) ) ;
#9590 = FACE_OUTER_BOUND ( 'NONE', #15607, .T. ) ;
#9591 = ORIENTED_EDGE ( 'NONE', *, *, #5000, .T. ) ;
#9592 = CARTESIAN_POINT ( 'NONE',  ( 6.500000000000005329, -4.484949146646330931, -3.631840208645857437 ) ) ;
#9593 = DIRECTION ( 'NONE',  ( -1.000000000000000000, 0.000000000000000000, 0.000000000000000000 ) ) ;
#9594 = ADVANCED_FACE ( 'NONE', ( #18103 ), #16306, .F. ) ;
#9595 = CIRCLE ( 'NONE', #10229, 1.000000000000000888 ) ;
#9596 = B_SPLINE_CURVE_WITH_KNOTS ( 'NONE', 3,
 ( #1590, #4983, #6180, #15501, #17193, #7879 ),
 .UNSPECIFIED., .F., .F.,
 ( 4, 2, 4 ),
 ( 4.462636793144160676E-07, 0.001879885123570646096, 0.003759323983461977832 ),
 .UNSPECIFIED. ) ;
#9597 = ADVANCED_FACE ( 'NONE', ( #5684 ), #156, .F. ) ;
#9598 = AXIS2_PLACEMENT_3D ( 'NONE', #319, #12631, #6400 ) ;
#9599 = DIRECTION ( 'NONE',  ( 0.000000000000000000, -0.6818181818181815457, -0.7315216790650493905 ) ) ;
#9600 = FACE_OUTER_BOUND ( 'NONE', #3240, .T. ) ;
#9601 = CARTESIAN_POINT ( 'NONE',  ( -7.937500000000000000, 4.582717761692651770, -6.527800000000000047 ) ) ;
#9602 = VERTEX_POINT ( 'NONE', #12494 ) ;
#9603 = CARTESIAN_POINT ( 'NONE',  ( 13.50000000000000533, 4.080749450109650844, 4.080749450109649956 ) ) ;
#9604 = CARTESIAN_POINT ( 'NONE',  ( 17.11901729331276556, 5.562305898749055011, -35.00000000000000000 ) ) ;
#9605 = CARTESIAN_POINT ( 'NONE',  ( 5.207209108562820710, -2.318398865532075526, 0.000000000000000000 ) ) ;
#9606 = EDGE_LOOP ( 'NONE', ( #16234, #1792, #18139, #9134 ) ) ;
#9607 = DIRECTION ( 'NONE',  ( 1.000000000000000000, 6.419766481290786633E-33, -0.000000000000000000 ) ) ;
#9608 = CARTESIAN_POINT ( 'NONE',  ( -5.626241948324210540, -16.73597674598852336, 32.00000000000000000 ) ) ;
#9609 = CARTESIAN_POINT ( 'NONE',  ( 6.000000000000005329, 4.936344801571308061, -2.849999999999988987 ) ) ;
#9610 = CARTESIAN_POINT ( 'NONE',  ( 4.762499999999999289, 0.000000000000000000, 0.000000000000000000 ) ) ;
#9611 = LINE ( 'NONE', #3404, #7618 ) ;
#9612 = ORIENTED_EDGE ( 'NONE', *, *, #14569, .F. ) ;
#9613 = CARTESIAN_POINT ( 'NONE',  ( -2.000000000000001776, 9.887492094615969966E-16, 8.073750000000021743 ) ) ;
#9614 = AXIS2_PLACEMENT_3D ( 'NONE', #16421, #11916, #4499 ) ;
#9615 = LINE ( 'NONE', #12809, #585 ) ;
#9616 = STYLED_ITEM ( 'NONE', ( #8810 ), #15810 ) ;
#9617 = ORIENTED_EDGE ( 'NONE', *, *, #11353, .F. ) ;
#9618 = CARTESIAN_POINT ( 'NONE',  ( 2.789999999999999147, -14.55412442567604003, -19.64056340710890325 ) ) ;
#9619 = EDGE_CURVE ( 'NONE', #3576, #14571, #4690, .T. ) ;
#9620 = DIRECTION ( 'NONE',  ( -1.000000000000000000, -0.000000000000000000, -0.000000000000000000 ) ) ;
#9621 = ORIENTED_EDGE ( 'NONE', *, *, #18502, .T. ) ;
#9622 = EDGE_CURVE ( 'NONE', #17426, #5986, #12954, .T. ) ;
#9623 = EDGE_CURVE ( 'NONE', #10783, #3731, #11217, .T. ) ;
#9624 = CARTESIAN_POINT ( 'NONE',  ( 1.039999999999996483, -12.96210679857803783, 24.89775460606827551 ) ) ;
#9625 = DIRECTION ( 'NONE',  ( -1.000000000000000000, -1.224646799147353207E-16, 0.000000000000000000 ) ) ;
#9626 =( BOUNDED_SURFACE ( )  B_SPLINE_SURFACE ( 1, 2, ( 
 ( #19005, #5192, #15909, #3695, #2292, #3795, #6681, #2389, #12906, #11500, #8297, #5296, #6878, #9815, #804, #18902, #11403 ),
 ( #9916, #8405, #14515, #16111, #16002, #14408, #13006, #8503, #17601, #19097, #606, #15477, #11068, #9377, #668, #15573, #15671 ) ),
 .UNSPECIFIED., .F., .F., .F. ) 
 B_SPLINE_SURFACE_WITH_KNOTS ( ( 2, 2 ),
 ( 3, 2, 2, 2, 2, 2, 2, 2, 3 ),
 ( 0.000000000000000000, 1.000000000000000000 ),
 ( 0.000000000000000000, 0.05000000000000000278, 0.1000000000000000056, 0.1499999999999999944, 0.2000000000000000111, 0.2500000000000000000, 0.2999999999999999889, 0.3499999999999999778, 0.4000000000000000222 ),
 .UNSPECIFIED. ) 
 GEOMETRIC_REPRESENTATION_ITEM ( )  RATIONAL_B_SPLINE_SURFACE ( (
 ( 1.000000000000000000, 0.9876883405951377704, 1.000000000000000000, 0.9876883405951377704, 1.000000000000000000, 0.9876883405951377704, 1.000000000000000000, 0.9876883405951377704, 1.000000000000000000, 0.9876883405951377704, 1.000000000000000000, 0.9876883405951377704, 1.000000000000000000, 0.9876883405951377704, 1.000000000000000000, 0.9876883405951377704, 1.000000000000000000),
 ( 1.000000000000000000, 0.9876883405951377704, 1.000000000000000000, 0.9876883405951377704, 1.000000000000000000, 0.9876883405951377704, 1.000000000000000000, 0.9876883405951377704, 1.000000000000000000, 0.9876883405951377704, 1.000000000000000000, 0.9876883405951377704, 1.000000000000000000, 0.9876883405951377704, 1.000000000000000000, 0.9876883405951377704, 1.000000000000000000) ) ) 
 REPRESENTATION_ITEM ( '' )  SURFACE ( )  );
#9627 = VERTEX_POINT ( 'NONE', #9400 ) ;
#9628 = AXIS2_PLACEMENT_3D ( 'NONE', #4694, #17098, #4891 ) ;
#9629 =( REPRESENTATION_RELATIONSHIP ('NONE','NONE', #18211, #14878 ) REPRESENTATION_RELATIONSHIP_WITH_TRANSFORMATION ( #2431 )SHAPE_REPRESENTATION_RELATIONSHIP( ) );
#9630 = CARTESIAN_POINT ( 'NONE',  ( 2.257825467309738876, -26.83036154824992536, -3.467596033028569114 ) ) ;
#9631 = CARTESIAN_POINT ( 'NONE',  ( -2.318398865532001363, 5.207209108562852684, -14.31249999590322552 ) ) ;
#9632 = DIRECTION ( 'NONE',  ( -1.000000000000000000, -0.000000000000000000, -0.000000000000000000 ) ) ;
#9633 = ORIENTED_EDGE ( 'NONE', *, *, #9342, .F. ) ;
#9634 = DIRECTION ( 'NONE',  ( 1.000000000000000000, 0.000000000000000000, 0.000000000000000000 ) ) ;
#9635 = EDGE_LOOP ( 'NONE', ( #2996, #13021, #18011, #13141 ) ) ;
#9636 = CARTESIAN_POINT ( 'NONE',  ( 2.783068888626319293, -22.53293026234510776, 9.685942809246967045 ) ) ;
#9637 = ORIENTED_EDGE ( 'NONE', *, *, #7613, .T. ) ;
#9638 = EDGE_CURVE ( 'NONE', #2241, #759, #12300, .T. ) ;
#9639 = CYLINDRICAL_SURFACE ( 'NONE', #13104, 1.000000000000002665 ) ;
#9640 = CARTESIAN_POINT ( 'NONE',  ( -16.68117051311640253, -3.372863662543042818, -32.00000000000000000 ) ) ;
#9641 = CARTESIAN_POINT ( 'NONE',  ( -16.19790265903627713, 9.644882309621941374, -32.00000000000000000 ) ) ;
#9642 = FACE_OUTER_BOUND ( 'NONE', #12965, .T. ) ;
#9643 = ORIENTED_EDGE ( 'NONE', *, *, #17258, .T. ) ;
#9644 = CARTESIAN_POINT ( 'NONE',  ( 2.789999999999999147, -20.62201879784921843, 12.52067188844344336 ) ) ;
#9645 = CYLINDRICAL_SURFACE ( 'NONE', #16814, 9.000000000000001776 ) ;
#9646 = AXIS2_PLACEMENT_3D ( 'NONE', #16356, #2638, #2738 ) ;
#9647 = VERTEX_POINT ( 'NONE', #12399 ) ;
#9648 = AXIS2_PLACEMENT_3D ( 'NONE', #18679, #4976, #17184 ) ;
#9649 = VECTOR ( 'NONE', #17437, 1000.000000000000000 ) ;
#9650 = CARTESIAN_POINT ( 'NONE',  ( 3.954556930911861112, 2.873153789725825913, -14.46874999795161720 ) ) ;
#9651 = EDGE_CURVE ( 'NONE', #14843, #1533, #1784, .T. ) ;
#9652 = DIRECTION ( 'NONE',  ( -1.000000000000000000, 0.000000000000000000, 0.000000000000000000 ) ) ;
#9653 = DIRECTION ( 'NONE',  ( 0.000000000000000000, 0.000000000000000000, 1.000000000000000000 ) ) ;
#9654 = EDGE_LOOP ( 'NONE', ( #13260, #8234 ) ) ;
#9655 = DIRECTION ( 'NONE',  ( -0.4999999999999977240, 0.7499999999999961142, 0.4330127018922284576 ) ) ;
#9656 = CARTESIAN_POINT ( 'NONE',  ( 14.84374999795161543, 4.861323657744413218, -0.5109457054261112852 ) ) ;
#9657 = ORIENTED_EDGE ( 'NONE', *, *, #1863, .T. ) ;
#9658 = FACE_OUTER_BOUND ( 'NONE', #3022, .T. ) ;
#9659 = CIRCLE ( 'NONE', #61, 1.000000000000004441 ) ;
#9660 = VERTEX_POINT ( 'NONE', #15399 ) ;
#9661 = PRODUCT_CONTEXT ( 'NONE', #17626, 'mechanical' ) ;
#9662 = CIRCLE ( 'NONE', #6741, 8.073750000000021743 ) ;
#9663 = DIRECTION ( 'NONE',  ( -1.000000000000000000, 0.000000000000000000, 0.000000000000000000 ) ) ;
#9664 = CARTESIAN_POINT ( 'NONE',  ( 2.789999999999999147, -19.91106274590524094, 14.18181402625735466 ) ) ;
#9665 = ORIENTED_EDGE ( 'NONE', *, *, #4613, .F. ) ;
#9666 = VERTEX_POINT ( 'NONE', #4888 ) ;
#9667 = CARTESIAN_POINT ( 'NONE',  ( 2.765633920072239516, -2.336989772644097574, -24.63872515616085224 ) ) ;
#9668 = CARTESIAN_POINT ( 'NONE',  ( 7.626241948324204323, -16.73597674598852691, 32.00000000000000000 ) ) ;
#9669 = EDGE_CURVE ( 'NONE', #3614, #10900, #19015, .T. ) ;
#9670 = ORIENTED_EDGE ( 'NONE', *, *, #13563, .T. ) ;
#9671 = AXIS2_PLACEMENT_3D ( 'NONE', #13581, #5870, #17994 ) ;
#9672 = EDGE_CURVE ( 'NONE', #8919, #2645, #13897, .T. ) ;
#9673 = CARTESIAN_POINT ( 'NONE',  ( -3.114526743279308896, -3.846120219227900705, -7.343749997951615427 ) ) ;
#9674 = TOROIDAL_SURFACE ( 'NONE', #17007, 6.000000000000000000, 1.199999999999999956 ) ;
#9675 = ORIENTED_EDGE ( 'NONE', *, *, #10431, .T. ) ;
#9676 = CIRCLE ( 'NONE', #15738, 1.000000000000004441 ) ;
#9677 = EDGE_CURVE ( 'NONE', #12952, #1346, #7629, .T. ) ;
#9678 = EDGE_CURVE ( 'NONE', #16866, #8277, #18061, .T. ) ;
#9679 = CIRCLE ( 'NONE', #17338, 9.000000000000000000 ) ;
#9680 = CYLINDRICAL_SURFACE ( 'NONE', #9902, 0.9999999999999974465 ) ;
#9681 = STYLED_ITEM ( 'NONE', ( #3966 ), #2634 ) ;
#9682 = DIRECTION ( 'NONE',  ( 0.000000000000000000, 0.8090169943749400128, 0.5877852522924831291 ) ) ;
#9683 = CARTESIAN_POINT ( 'NONE',  ( 0.1882239080259275332, 25.40949241676353410, 5.251266773802457877 ) ) ;
#9684 = VERTEX_POINT ( 'NONE', #17192 ) ;
#9685 = LINE ( 'NONE', #18769, #5648 ) ;
#9686 =( LENGTH_UNIT ( ) NAMED_UNIT ( * ) SI_UNIT ( .MILLI., .METRE. ) );
#9687 = CARTESIAN_POINT ( 'NONE',  ( -16.96448111170888851, 1.130229351527647808, -32.00000000000000000 ) ) ;
#9688 = ORIENTED_EDGE ( 'NONE', *, *, #2465, .F. ) ;
#9689 = VERTEX_POINT ( 'NONE', #13696 ) ;
#9690 = CARTESIAN_POINT ( 'NONE',  ( -5.574407415329178939, -1.493657965219446382, -8.500000000000007105 ) ) ;
#9691 = CIRCLE ( 'NONE', #1366, 2.524999999999995914 ) ;
#9692 = CIRCLE ( 'NONE', #15755, 4.824999999999999289 ) ;
#9693 = CARTESIAN_POINT ( 'NONE',  ( 0.000000000000000000, -23.48180575137727288, -5.535312321042949790 ) ) ;
#9694 = AXIS2_PLACEMENT_3D ( 'NONE', #18447, #7833, #18255 ) ;
#9695 = CARTESIAN_POINT ( 'NONE',  ( -3.350375938067097437, 4.611396867937201272, -9.000000000000005329 ) ) ;
#9696 = VERTEX_POINT ( 'NONE', #6079 ) ;
#9697 = DIRECTION ( 'NONE',  ( 1.000000000000000000, 0.000000000000000000, 0.000000000000000000 ) ) ;
#9698 = CIRCLE ( 'NONE', #3611, 6.760799999999997034 ) ;
#9699 = DIRECTION ( 'NONE',  ( 0.000000000000000000, 0.000000000000000000, -1.000000000000000000 ) ) ;
#9700 = VERTEX_POINT ( 'NONE', #12197 ) ;
#9701 = DIRECTION ( 'NONE',  ( -0.5000000000000009992, -0.8660254037844380415, 0.000000000000000000 ) ) ;
#9702 = ADVANCED_FACE ( 'NONE', ( #1588 ), #90, .T. ) ;
#9703 = EDGE_CURVE ( 'NONE', #14603, #7952, #4318, .T. ) ;
#9704 = DIRECTION ( 'NONE',  ( 1.000000000000000000, 0.000000000000000000, 0.000000000000000000 ) ) ;
#9705 = STYLED_ITEM ( 'NONE', ( #12725 ), #12355 ) ;
#9706 = CARTESIAN_POINT ( 'NONE',  ( 0.000000000000000000, 0.000000000000000000, -32.00000000000000000 ) ) ;
#9707 = DIRECTION ( 'NONE',  ( 1.000000000000000000, 0.000000000000000000, 0.000000000000000000 ) ) ;
#9708 = CARTESIAN_POINT ( 'NONE',  ( -2.620002426024580000, -5.142044285764733935, -12.50000000000000533 ) ) ;
#9709 = PRODUCT ( 'short pitch roller chain wheel_s_iso_Chain wheel ISO - 20Z 05B-1 --20SA8.0N', 'short pitch roller chain wheel_s_iso_Chain wheel ISO - 20Z 05B-1 --20SA8.0N', '', ( #6426 ) ) ;
#9710 = DIRECTION ( 'NONE',  ( 1.000000000000000000, 0.000000000000000000, 0.000000000000000000 ) ) ;
#9711 = CYLINDRICAL_SURFACE ( 'NONE', #17417, 4.200000000000000178 ) ;
#9712 = CIRCLE ( 'NONE', #4271, 3.323500000000020993 ) ;
#9713 = VERTEX_POINT ( 'NONE', #5467 ) ;
#9714 = ADVANCED_FACE ( 'NONE', ( #590 ), #15893, .T. ) ;
#9715 = CARTESIAN_POINT ( 'NONE',  ( -7.682766964941417370E-14, -9.515416771311052457, -22.38018801136486502 ) ) ;
#9716 =( LENGTH_UNIT ( ) NAMED_UNIT ( * ) SI_UNIT ( .MILLI., .METRE. ) );
#9717 = CARTESIAN_POINT ( 'NONE',  ( 2.444050593750020095, 4.233219804643871598, -6.843749997951615427 ) ) ;
#9718 = LINE ( 'NONE', #15611, #9195 ) ;
#9719 = CYLINDRICAL_SURFACE ( 'NONE', #8284, 4.000000000000000000 ) ;
#9720 = ORIENTED_EDGE ( 'NONE', *, *, #12742, .T. ) ;
#9721 = CARTESIAN_POINT ( 'NONE',  ( -7.680503837993603605E-14, 23.69897269326676437, 5.456611084821939350 ) ) ;
#9722 = EDGE_CURVE ( 'NONE', #7172, #16673, #16095, .T. ) ;
#9723 = STYLED_ITEM ( 'NONE', ( #695 ), #5887 ) ;
#9724 = DIRECTION ( 'NONE',  ( -1.000000000000000000, 0.000000000000000000, 0.000000000000000000 ) ) ;
#9725 = ADVANCED_FACE ( 'NONE', ( #9900, #11188 ), #13083, .T. ) ;
#9726 = ORIENTED_EDGE ( 'NONE', *, *, #13709, .F. ) ;
#9727 = CARTESIAN_POINT ( 'NONE',  ( 13.31249999590322730, -5.421022142882365280, -1.761396867937238042 ) ) ;
#9728 = DIRECTION ( 'NONE',  ( 0.000000000000000000, 0.000000000000000000, -1.000000000000000000 ) ) ;
#9729 = VERTEX_POINT ( 'NONE', #19177 ) ;
#9730 = VECTOR ( 'NONE', #6770, 1000.000000000000000 ) ;
#9731 = DIRECTION ( 'NONE',  ( 0.000000000000000000, 0.000000000000000000, 1.000000000000000000 ) ) ;
#9732 = CARTESIAN_POINT ( 'NONE',  ( 13.00000000000000178, 4.568735188514060575, 1.737869959597756697 ) ) ;
#9733 = EDGE_LOOP ( 'NONE', ( #4948, #4421 ) ) ;
#9734 =( GEOMETRIC_REPRESENTATION_CONTEXT ( 3 ) GLOBAL_UNCERTAINTY_ASSIGNED_CONTEXT ( ( #19002 ) ) GLOBAL_UNIT_ASSIGNED_CONTEXT ( ( #13091, #12997, #14790 ) ) REPRESENTATION_CONTEXT ( 'NONE', 'WORKASPACE' ) );
#9735 = AXIS2_PLACEMENT_3D ( 'NONE', #5669, #1178, #7058 ) ;
#9736 = CARTESIAN_POINT ( 'NONE',  ( 1.394999999999999574, 27.76164181293051669, -4.147968289691385202 ) ) ;
#9737 =( NAMED_UNIT ( * ) SI_UNIT ( $, .STERADIAN. ) SOLID_ANGLE_UNIT ( ) );
#9738 = DIRECTION ( 'NONE',  ( 1.000000000000000000, 0.000000000000000000, 0.000000000000000000 ) ) ;
#9739 = VERTEX_POINT ( 'NONE', #8281 ) ;
#9740 = LINE ( 'NONE', #13117, #5 ) ;
#9741 = ORIENTED_EDGE ( 'NONE', *, *, #3012, .F. ) ;
#9742 = CARTESIAN_POINT ( 'NONE',  ( 3.143139765844590983, -4.840010801796506001, -13.81249999590322730 ) ) ;
#9743 = EDGE_LOOP ( 'NONE', ( #15561, #18754, #2463, #5357 ) ) ;
#9744 = DIRECTION ( 'NONE',  ( -1.000000000000000000, 0.000000000000000000, 0.000000000000000000 ) ) ;
#9745 = AXIS2_PLACEMENT_3D ( 'NONE', #419, #14425, #17226 ) ;
#9746 = DIRECTION ( 'NONE',  ( 0.000000000000000000, 0.000000000000000000, -1.000000000000000000 ) ) ;
#9747 = LINE ( 'NONE', #14435, #64 ) ;
#9748 = CARTESIAN_POINT ( 'NONE',  ( 3.114526743279282694, 3.846120219227923798, -7.343749997951615427 ) ) ;
#9749 = ORIENTED_EDGE ( 'NONE', *, *, #19676, .F. ) ;
#9750 = FACE_BOUND ( 'NONE', #9439, .T. ) ;
#9751 = CARTESIAN_POINT ( 'NONE',  ( 2.789999999999999147, 9.324097380959445402, 22.25075486061742325 ) ) ;
#9752 = CIRCLE ( 'NONE', #1108, 1.000000000000000888 ) ;
#9753 = ORIENTED_EDGE ( 'NONE', *, *, #5643, .F. ) ;
#9754 =( BOUNDED_CURVE ( )  B_SPLINE_CURVE ( 2, ( #1996, #17111, #12414, #3402, #7695, #8095, #6192, #6287, #18507, #1708, #4997 ),
 .UNSPECIFIED., .F., .F. ) 
 B_SPLINE_CURVE_WITH_KNOTS ( ( 3, 2, 2, 2, 2, 3 ),
 ( 0.1666819079834116757, 0.2000000000000000111, 0.2500000000000000000, 0.2999999999999999889, 0.3499999999999999778, 0.4000000000000000222 ),
 .UNSPECIFIED. ) 
 CURVE ( )  GEOMETRIC_REPRESENTATION_ITEM ( )  RATIONAL_B_SPLINE_CURVE ( ( 0.9945256517182512468, 0.9917959799814380917, 1.000000000000000000, 0.9876883405951377704, 1.000000000000000000, 0.9876883405951377704, 1.000000000000000000, 0.9876883405951377704, 1.000000000000000000, 0.9876883405951377704, 1.000000000000000000 ) ) 
 REPRESENTATION_ITEM ( '' )  );
#9755 = CARTESIAN_POINT ( 'NONE',  ( -17.96448111170888851, 1.130229351527647585, -32.00000000000000000 ) ) ;
#9756 = AXIS2_PLACEMENT_3D ( 'NONE', #6672, #12798, #295 ) ;
#9757 = DIRECTION ( 'NONE',  ( -1.000000000000000000, -0.000000000000000000, -0.000000000000000000 ) ) ;
#9758 = CARTESIAN_POINT ( 'NONE',  ( -4.942249507334558700, -0.2590123213420630899, -12.96874999795161543 ) ) ;
#9759 = ORIENTED_EDGE ( 'NONE', *, *, #6001, .F. ) ;
#9760 = CARTESIAN_POINT ( 'NONE',  ( 0.1855657168891852171, 22.53097606933003405, -12.84444904262000975 ) ) ;
#9761 = CARTESIAN_POINT ( 'NONE',  ( 14.81249999590322552, 5.574407415329178939, -1.493657965219446382 ) ) ;
#9762 = CARTESIAN_POINT ( 'NONE',  ( 2.999999999999998224, -3.950217066951267064, 3.681818181818180769 ) ) ;
#9763 = ORIENTED_EDGE ( 'NONE', *, *, #13771, .F. ) ;
#9764 = DIRECTION ( 'NONE',  ( 0.000000000000000000, 1.000000000000000000, -0.000000000000000000 ) ) ;
#9765 = TOROIDAL_SURFACE ( 'NONE', #1123, 6.200000000000021494, 0.2000000000000003164 ) ;
#9766 = EDGE_LOOP ( 'NONE', ( #16634, #6594, #2971, #5999 ) ) ;
#9767 = CONTEXT_DEPENDENT_SHAPE_REPRESENTATION ( #3483, #14822 ) ;
#9768 = CARTESIAN_POINT ( 'NONE',  ( 12.84374999795161543, -3.632567103900546712, 3.270778111535314281 ) ) ;
#9769 = CARTESIAN_POINT ( 'NONE',  ( 1.394999999999999574, 27.76164181293051669, 4.147968289691385202 ) ) ;
#9770 = B_SPLINE_CURVE_WITH_KNOTS ( 'NONE', 1,
 ( #11719, #5700 ),
 .UNSPECIFIED., .F., .F.,
 ( 2, 2 ),
 ( 0.000000000000000000, 1.000000000000000000 ),
 .UNSPECIFIED. ) ;
#9771 = ORIENTED_EDGE ( 'NONE', *, *, #15518, .F. ) ;
#9772 = ORIENTED_EDGE ( 'NONE', *, *, #9442, .T. ) ;
#9773 = CARTESIAN_POINT ( 'NONE',  ( 0.02436607992775934733, -21.30679549418640306, 12.59161484032904887 ) ) ;
#9774 = CARTESIAN_POINT ( 'NONE',  ( 0.000000000000000000, -7.909232158574647009, -21.81711360614308148 ) ) ;
#9775 = CARTESIAN_POINT ( 'NONE',  ( 6.468749997951615427, 4.233219804643887585, -2.444050593749990341 ) ) ;
#9776 = ADVANCED_FACE ( 'NONE', ( #882 ), #15507, .T. ) ;
#9777 = ORIENTED_EDGE ( 'NONE', *, *, #6631, .T. ) ;
#9778 =( LENGTH_UNIT ( ) NAMED_UNIT ( * ) SI_UNIT ( .MILLI., .METRE. ) );
#9779 = CIRCLE ( 'NONE', #12639, 9.000000000000001776 ) ;
#9780 = ORIENTED_EDGE ( 'NONE', *, *, #17071, .T. ) ;
#9781 = AXIS2_PLACEMENT_3D ( 'NONE', #15942, #8233, #637 ) ;
#9782 = CARTESIAN_POINT ( 'NONE',  ( 10.58013454126452046, -14.56230589874905412, -35.00000000000000000 ) ) ;
#9783 = CARTESIAN_POINT ( 'NONE',  ( 8.500000000000005329, -4.080749450109678378, 4.080749450109622423 ) ) ;
#9784 = EDGE_CURVE ( 'NONE', #8006, #10318, #17392, .T. ) ;
#9785 = CARTESIAN_POINT ( 'NONE',  ( -5.476417968967388639, 17.43449690031536292, -35.00000000000000000 ) ) ;
#9786 = VERTEX_POINT ( 'NONE', #5076 ) ;
#9787 = CARTESIAN_POINT ( 'NONE',  ( 0.1882239034349769691, -22.54313264455003463, -12.84621645676869939 ) ) ;
#9788 = CARTESIAN_POINT ( 'NONE',  ( 1.039999999999997593, -24.89775460606841051, 12.96210679857778025 ) ) ;
#9789 = ORIENTED_EDGE ( 'NONE', *, *, #12270, .F. ) ;
#9790 = ORIENTED_EDGE ( 'NONE', *, *, #18465, .F. ) ;
#9791 = CARTESIAN_POINT ( 'NONE',  ( -3.846120219227901593, 3.114526743279308896, -11.96874999795161365 ) ) ;
#9792 = AXIS2_PLACEMENT_3D ( 'NONE', #7124, #16346, #19440 ) ;
#9793 = EDGE_CURVE ( 'NONE', #5905, #9786, #16194, .T. ) ;
#9794 = DIRECTION ( 'NONE',  ( -1.000000000000000000, -0.000000000000000000, -0.000000000000000000 ) ) ;
#9795 = CARTESIAN_POINT ( 'NONE',  ( 0.07181525480391370841, -12.74223776959215826, 21.92234060054341427 ) ) ;
#9796 = ORIENTED_EDGE ( 'NONE', *, *, #15421, .T. ) ;
#9797 = CARTESIAN_POINT ( 'NONE',  ( 11.46874999795161543, 2.444050593750049405, -4.233219804643852946 ) ) ;
#9798 = CARTESIAN_POINT ( 'NONE',  ( 13.00000000000000178, -3.908719486245979091, 2.935207862670018653 ) ) ;
#9799 = ORIENTED_EDGE ( 'NONE', *, *, #17074, .F. ) ;
#9800 = PLANE ( 'NONE',  #16463 ) ;
#9801 = DIRECTION ( 'NONE',  ( 0.000000000000000000, 0.000000000000000000, -1.000000000000000000 ) ) ;
#9802 = AXIS2_PLACEMENT_3D ( 'NONE', #524, #10826, #3118 ) ;
#9803 = TOROIDAL_SURFACE ( 'NONE', #3724, 24.12539914357697413, 8.000000000000000000 ) ;
#9804 = CARTESIAN_POINT ( 'NONE',  ( 2.789999999999999147, -1.991882183130462503, 24.04302995059964942 ) ) ;
#9805 = FACE_OUTER_BOUND ( 'NONE', #14948, .T. ) ;
#9806 = EDGE_CURVE ( 'NONE', #941, #15571, #5373, .T. ) ;
#9807 = DIRECTION ( 'NONE',  ( 0.000000000000000000, 0.000000000000000000, -1.000000000000000000 ) ) ;
#9808 = DIRECTION ( 'NONE',  ( 0.000000000000000000, -1.000000000000000000, 0.000000000000000000 ) ) ;
#9809 = CARTESIAN_POINT ( 'NONE',  ( 0.02436607992776281678, 2.336989772644269436, 24.63872515616083447 ) ) ;
#9810 = ORIENTED_EDGE ( 'NONE', *, *, #14618, .F. ) ;
#9811 = DIRECTION ( 'NONE',  ( -0.8660254037844398178, 6.047423072554923456E-15, 0.4999999999999979461 ) ) ;
#9812 = EDGE_CURVE ( 'NONE', #9108, #18640, #8481, .T. ) ;
#9813 = CARTESIAN_POINT ( 'NONE',  ( -20.63749999999999929, 0.000000000000000000, -5.200000000000000178 ) ) ;
#9814 = CARTESIAN_POINT ( 'NONE',  ( 4.840010801796506890, 3.143139765844590983, -8.812499995903225525 ) ) ;
#9815 = CARTESIAN_POINT ( 'NONE',  ( 13.34374999795161365, -0.2590123213420631454, -4.942249507334558700 ) ) ;
#9816 = VERTEX_POINT ( 'NONE', #688 ) ;
#9817 = EDGE_CURVE ( 'NONE', #12686, #7114, #6766, .T. ) ;
#9818 = CARTESIAN_POINT ( 'NONE',  ( -11.00000000000000355, -5.400000000000001243, 0.000000000000000000 ) ) ;
#9819 = AXIS2_PLACEMENT_3D ( 'NONE', #17496, #10098, #9710 ) ;
#9820 = CARTESIAN_POINT ( 'NONE',  ( -5.700000000000001066, 0.000000000000000000, -7.312499995903225525 ) ) ;
#9821 = AXIS2_PLACEMENT_3D ( 'NONE', #1776, #6356, #15489 ) ;
#9822 = EDGE_LOOP ( 'NONE', ( #14839, #8205, #9238, #4291 ) ) ;
#9823 = CARTESIAN_POINT ( 'NONE',  ( 10.31249999590322552, -4.611396867937225252, 3.350375938067065462 ) ) ;
#9824 = DIRECTION ( 'NONE',  ( 1.000000000000000000, 0.000000000000000000, 0.000000000000000000 ) ) ;
#9825 = ORIENTED_EDGE ( 'NONE', *, *, #6240, .T. ) ;
#9826 = CARTESIAN_POINT ( 'NONE',  ( -4.611396867937226141, -3.350375938067064574, 0.000000000000000000 ) ) ;
#9827 = EDGE_CURVE ( 'NONE', #8532, #9982, #6562, .T. ) ;
#9828 = FACE_OUTER_BOUND ( 'NONE', #14495, .T. ) ;
#9829 = CARTESIAN_POINT ( 'NONE',  ( -30.00000000000000000, -1.925929944387235853E-31, 0.000000000000000000 ) ) ;
#9830 = DIRECTION ( 'NONE',  ( 1.000000000000000000, 6.419766481290786633E-33, -0.000000000000000000 ) ) ;
#9831 = VERTEX_POINT ( 'NONE', #15792 ) ;
#9832 = DIRECTION ( 'NONE',  ( 0.000000000000000000, 0.000000000000000000, 1.000000000000000000 ) ) ;
#9833 = DIRECTION ( 'NONE',  ( 0.000000000000000000, 0.000000000000000000, 1.000000000000000000 ) ) ;
#9834 = ADVANCED_FACE ( 'NONE', ( #14289 ), #9800, .F. ) ;
#9835 = LINE ( 'NONE', #4921, #1429 ) ;
#9836 = CIRCLE ( 'NONE', #19391, 28.06981291497571362 ) ;
#9837 = EDGE_CURVE ( 'NONE', #677, #12799, #17438, .T. ) ;
#9838 = ORIENTED_EDGE ( 'NONE', *, *, #4370, .T. ) ;
#9839 = CARTESIAN_POINT ( 'NONE',  ( 0.02436607992776455150, 5.391175441198956086, -24.15498966839956907 ) ) ;
#9840 = ORIENTED_EDGE ( 'NONE', *, *, #6094, .F. ) ;
#9841 = CARTESIAN_POINT ( 'NONE',  ( 13.00000000000000178, 0.000000000000000000, 0.000000000000000000 ) ) ;
#9842 = ORIENTED_EDGE ( 'NONE', *, *, #5159, .T. ) ;
#9843 = APPLICATION_CONTEXT ( 'automotive_design' ) ;
#9844 = LINE ( 'NONE', #15933, #17578 ) ;
#9845 = CARTESIAN_POINT ( 'NONE',  ( 1.761396867937200073, 5.421022142882376826, -13.31249999590322730 ) ) ;
#9846 = DIRECTION ( 'NONE',  ( -1.000000000000000000, -0.000000000000000000, 0.000000000000000000 ) ) ;
#9847 = EDGE_CURVE ( 'NONE', #15, #13643, #5278, .T. ) ;
#9848 = CARTESIAN_POINT ( 'NONE',  ( 4.150607464521812062, 2.695436003842704764, -8.343749997951611874 ) ) ;
#9849 = EDGE_LOOP ( 'NONE', ( #14208, #10384, #8010, #5818 ) ) ;
#9850 = FACE_OUTER_BOUND ( 'NONE', #14936, .T. ) ;
#9851 = DIRECTION ( 'NONE',  ( 9.559896011775280412E-17, 0.7806247497997995666, -0.6250000000000001110 ) ) ;
#9852 = CIRCLE ( 'NONE', #13341, 1.000000000000004441 ) ;
#9853 = EDGE_LOOP ( 'NONE', ( #623, #2553, #16628, #15986, #12069, #13558 ) ) ;
#9854 = CIRCLE ( 'NONE', #13973, 28.06981291497571362 ) ;
#9855 = EDGE_CURVE ( 'NONE', #19204, #4306, #13585, .T. ) ;
#9856 = DIRECTION ( 'NONE',  ( 0.000000000000000000, 0.000000000000000000, -1.000000000000000000 ) ) ;
#9857 = DIRECTION ( 'NONE',  ( 0.000000000000000000, 0.000000000000000000, 1.000000000000000000 ) ) ;
#9858 = CARTESIAN_POINT ( 'NONE',  ( -17.11901729331276911, 5.562305898749051458, 32.00000000000000000 ) ) ;
#9859 = EDGE_CURVE ( 'NONE', #5986, #17426, #9779, .T. ) ;
#9860 = ORIENTED_EDGE ( 'NONE', *, *, #5657, .F. ) ;
#9861 = LINE ( 'NONE', #15951, #19655 ) ;
#9862 = DIRECTION ( 'NONE',  ( 1.000000000000000000, 0.000000000000000000, 0.000000000000000000 ) ) ;
#9863 = CARTESIAN_POINT ( 'NONE',  ( 0.000000000000000000, 0.000000000000000000, 0.000000000000000000 ) ) ;
#9864 = ORIENTED_EDGE ( 'NONE', *, *, #13001, .T. ) ;
#9865 = CARTESIAN_POINT ( 'NONE',  ( 0.000000000000000000, 12.52067188844379864, -20.62201879784900882 ) ) ;
#9866 = VECTOR ( 'NONE', #9811, 1000.000000000000000 ) ;
#9867 = ORIENTED_EDGE ( 'NONE', *, *, #10663, .F. ) ;
#9868 = ITEM_DEFINED_TRANSFORMATION ( 'NONE', 'NONE', #19450,  #16724 ) ;
#9869 =( LENGTH_UNIT ( ) NAMED_UNIT ( * ) SI_UNIT ( .MILLI., .METRE. ) );
#9870 = AXIS2_PLACEMENT_3D ( 'NONE', #14728, #16142, #16427 ) ;
#9871 = DIRECTION ( 'NONE',  ( -1.000000000000000000, -0.000000000000000000, -0.000000000000000000 ) ) ;
#9872 = ORIENTED_EDGE ( 'NONE', *, *, #9426, .T. ) ;
#9873 = ORIENTED_EDGE ( 'NONE', *, *, #3289, .F. ) ;
#9874 = CARTESIAN_POINT ( 'NONE',  ( 0.006930995026448713570, 5.408431875071442185, 23.92277630352796791 ) ) ;
#9875 = DIRECTION ( 'NONE',  ( -1.000000000000000000, 0.000000000000000000, 0.000000000000000000 ) ) ;
#9876 = LINE ( 'NONE', #15866, #12394 ) ;
#9877 = ORIENTED_EDGE ( 'NONE', *, *, #14920, .T. ) ;
#9878 = DIRECTION ( 'NONE',  ( 1.000000000000000000, 0.000000000000000000, 0.000000000000000000 ) ) ;
#9879 = EDGE_CURVE ( 'NONE', #3823, #11476, #16158, .T. ) ;
#9880 = AXIS2_PLACEMENT_3D ( 'NONE', #18072, #8964, #10472 ) ;
#9881 = ORIENTED_EDGE ( 'NONE', *, *, #5736, .F. ) ;
#9882 = DIRECTION ( 'NONE',  ( 0.000000000000000000, 0.000000000000000000, -1.000000000000000000 ) ) ;
#9883 = EDGE_CURVE ( 'NONE', #17326, #1519, #323, .T. ) ;
#9884 = CARTESIAN_POINT ( 'NONE',  ( 18.11901729331276911, 5.562305898749055011, -32.00000000000000000 ) ) ;
#9885 = CARTESIAN_POINT ( 'NONE',  ( -4.150607464521828938, -2.695436003842674566, -7.968749997951616315 ) ) ;
#9886 = ORIENTED_EDGE ( 'NONE', *, *, #607, .T. ) ;
#9887 =( NAMED_UNIT ( * ) PLANE_ANGLE_UNIT ( ) SI_UNIT ( $, .RADIAN. ) );
#9888 = CARTESIAN_POINT ( 'NONE',  ( 3.846120219227944670, 3.114526743279255161, -10.96874999795161720 ) ) ;
#9889 = ORIENTED_EDGE ( 'NONE', *, *, #6366, .T. ) ;
#9890 = ORIENTED_EDGE ( 'NONE', *, *, #17541, .T. ) ;
#9891 = LINE ( 'NONE', #8479, #18161 ) ;
#9892 = EDGE_CURVE ( 'NONE', #2502, #15630, #19334, .T. ) ;
#9893 = CARTESIAN_POINT ( 'NONE',  ( 13.00000000000000178, 3.789407127742559833, -3.087705756618140285 ) ) ;
#9894 = DIRECTION ( 'NONE',  ( 0.000000000000000000, 0.000000000000000000, 1.000000000000000000 ) ) ;
#9895 = PRODUCT_DEFINITION_FORMATION_WITH_SPECIFIED_SOURCE ( 'ANY', '', #19444, .NOT_KNOWN. ) ;
#9896 = VERTEX_POINT ( 'NONE', #17782 ) ;
#9897 = DIRECTION ( 'NONE',  ( 0.000000000000000000, 0.000000000000000000, 1.000000000000000000 ) ) ;
#9898 = CARTESIAN_POINT ( 'NONE',  ( -16.11901729331276911, 5.562305898749051458, 35.00000000000000000 ) ) ;
#9899 = ORIENTED_EDGE ( 'NONE', *, *, #14085, .F. ) ;
#9900 = FACE_BOUND ( 'NONE', #5410, .T. ) ;
#9901 = FACE_OUTER_BOUND ( 'NONE', #6031, .T. ) ;
#9902 = AXIS2_PLACEMENT_3D ( 'NONE', #10075, #17859, #11656 ) ;
#9903 = EDGE_CURVE ( 'NONE', #14221, #1705, #16067, .T. ) ;
#9904 = FACE_OUTER_BOUND ( 'NONE', #14091, .T. ) ;
#9905 = CARTESIAN_POINT ( 'NONE',  ( 15.28688694438835505, -7.664027248171309203, 35.00000000000000000 ) ) ;
#9906 = CARTESIAN_POINT ( 'NONE',  ( 10.34374999795161543, 4.150607464521792522, 2.695436003842732298 ) ) ;
#9907 = FACE_OUTER_BOUND ( 'NONE', #8098, .T. ) ;
#9908 = SURFACE_STYLE_USAGE ( .BOTH. , #4086 ) ;
#9909 = DIRECTION ( 'NONE',  ( 0.000000000000000000, 0.000000000000000000, 1.000000000000000000 ) ) ;
#9910 = B_SPLINE_CURVE_WITH_KNOTS ( 'NONE', 3,
 ( #19232, #5526, #11634, #748, #17737, #6824 ),
 .UNSPECIFIED., .F., .F.,
 ( 4, 2, 4 ),
 ( 0.008176170726434978109, 0.01049421029328159553, 0.01281224986012821296 ),
 .UNSPECIFIED. ) ;
#9911 = LINE ( 'NONE', #12901, #6387 ) ;
#9912 = ORIENTED_EDGE ( 'NONE', *, *, #5392, .T. ) ;
#9913 = CARTESIAN_POINT ( 'NONE',  ( 11.81249999590322552, 3.631840208645794821, 4.484949146646379781 ) ) ;
#9914 = CARTESIAN_POINT ( 'NONE',  ( 1.749999999999998002, 4.633866840648922292, 27.68468304288260384 ) ) ;
#9915 = DIRECTION ( 'NONE',  ( 1.000000000000000000, 0.000000000000000000, 0.000000000000000000 ) ) ;
#9916 = CARTESIAN_POINT ( 'NONE',  ( 6.468749997951615427, -4.233219804643904460, 2.444050593749960587 ) ) ;
#9917 = CARTESIAN_POINT ( 'NONE',  ( 0.02436607992776758727, 24.15498966839963302, 5.391175441198700291 ) ) ;
#9918 = CARTESIAN_POINT ( 'NONE',  ( -4.781284448697201483, -1.016293382781378485, -12.84374999795161543 ) ) ;
#9919 = ORIENTED_EDGE ( 'NONE', *, *, #17579, .T. ) ;
#9920 = CARTESIAN_POINT ( 'NONE',  ( 9.312499995903225525, -3.350375938067129855, 4.611396867937178179 ) ) ;
#9921 = EDGE_CURVE ( 'NONE', #18135, #17337, #11777, .T. ) ;
#9922 = ADVANCED_FACE ( 'NONE', ( #5664 ), #13184, .F. ) ;
#9923 = CARTESIAN_POINT ( 'NONE',  ( 2.500000000000002220, 0.000000000000000000, 0.000000000000000000 ) ) ;
#9924 = AXIS2_PLACEMENT_3D ( 'NONE', #829, #3915, #16227 ) ;
#9925 = ORIENTED_EDGE ( 'NONE', *, *, #6341, .T. ) ;
#9926 = DIRECTION ( 'NONE',  ( 0.000000000000000000, 0.000000000000000000, -1.000000000000000000 ) ) ;
#9927 = CIRCLE ( 'NONE', #12153, 4.000000000000000000 ) ;
#9928 = CARTESIAN_POINT ( 'NONE',  ( 0.5321745407694753460, 4.993157874728185952, -26.58873630738046501 ) ) ;
#9929 = DIRECTION ( 'NONE',  ( 0.000000000000000000, 1.000000000000000000, 0.000000000000000000 ) ) ;
#9930 = CARTESIAN_POINT ( 'NONE',  ( -5.700000000000001954, 6.980486755139915080E-16, 0.000000000000000000 ) ) ;
#9931 = ORIENTED_EDGE ( 'NONE', *, *, #2547, .T. ) ;
#9932 = CARTESIAN_POINT ( 'NONE',  ( 91.50000000000000000, 0.000000000000000000, 0.000000000000000000 ) ) ;
#9933 =( LENGTH_UNIT ( ) NAMED_UNIT ( * ) SI_UNIT ( .MILLI., .METRE. ) );
#9934 = CARTESIAN_POINT ( 'NONE',  ( 11.06250000000000000, 4.774285546475956322E-16, -3.797000000000000597 ) ) ;
#9935 = ORIENTED_EDGE ( 'NONE', *, *, #12199, .T. ) ;
#9936 = CARTESIAN_POINT ( 'NONE',  ( -6.626241948324210540, -16.73597674598852336, -32.00000000000000000 ) ) ;
#9937 = ORIENTED_EDGE ( 'NONE', *, *, #222, .F. ) ;
#9938 = DIRECTION ( 'NONE',  ( 1.000000000000000000, 0.000000000000000000, 0.000000000000000000 ) ) ;
#9939 = ORIENTED_EDGE ( 'NONE', *, *, #3212, .T. ) ;
#9940 = CIRCLE ( 'NONE', #17272, 9.500000000000000000 ) ;
#9941 = COLOUR_RGB ( '', 0.72549020, 0.75294118, 0.79215686) ;
#9942 = DIRECTION ( 'NONE',  ( -0.8191520442889898002, 1.003171929053522282E-16, 0.5735764363510488240 ) ) ;
#9943 = CARTESIAN_POINT ( 'NONE',  ( -7.937500000000000000, 4.582717761692651770, -6.527800000000000047 ) ) ;
#9944 = CARTESIAN_POINT ( 'NONE',  ( 2.601776121706765199, 17.47009390565519382, -19.18368891937472043 ) ) ;
#9945 = DIRECTION ( 'NONE',  ( -7.861946472586228936E-49, 1.224646799147353207E-16, 1.000000000000000000 ) ) ;
#9946 = EDGE_LOOP ( 'NONE', ( #18551, #4813, #16973, #12179, #13079, #18330, #2527, #5697 ) ) ;
#9947 = CARTESIAN_POINT ( 'NONE',  ( 0.02436607992775978102, 24.63872515616082737, 2.336989772644355146 ) ) ;
#9948 = PRODUCT_RELATED_PRODUCT_CATEGORY ( 'part', '', ( #2666 ) ) ;
#9949 = ORIENTED_EDGE ( 'NONE', *, *, #4420, .T. ) ;
#9950 = VECTOR ( 'NONE', #5938, 1000.000000000000000 ) ;
#9951 = EDGE_CURVE ( 'NONE', #12919, #1763, #15188, .T. ) ;
#9952 = CARTESIAN_POINT ( 'NONE',  ( 1.999999999999999112, 8.073750000000021743, 0.000000000000000000 ) ) ;
#9953 = CARTESIAN_POINT ( 'NONE',  ( -0.9027913098498961952, -5.699999999999994849, -12.81249999590322552 ) ) ;
#9954 = ADVANCED_FACE ( 'NONE', ( #19471 ), #15837, .T. ) ;
#9955 = EDGE_LOOP ( 'NONE', ( #16460, #7523, #1343, #4063 ) ) ;
#9956 = DIRECTION ( 'NONE',  ( 0.000000000000000000, 0.000000000000000000, -1.000000000000000000 ) ) ;
#9957 = CARTESIAN_POINT ( 'NONE',  ( -0.7741991708319226895, -4.888101187499994893, -11.96874999795161365 ) ) ;
#9958 = CARTESIAN_POINT ( 'NONE',  ( 5.700000000000002842, 2.725425358843983450E-16, -10.64522241986047568 ) ) ;
#9959 = ORIENTED_EDGE ( 'NONE', *, *, #14486, .F. ) ;
#9960 = DIRECTION ( 'NONE',  ( -1.000000000000000000, 0.000000000000000000, 0.000000000000000000 ) ) ;
#9961 = ORIENTED_EDGE ( 'NONE', *, *, #15150, .F. ) ;
#9962 = CONTEXT_DEPENDENT_SHAPE_REPRESENTATION ( #15878, #5378 ) ;
#9963 = DIRECTION ( 'NONE',  ( -0.000000000000000000, -0.000000000000000000, 1.000000000000000000 ) ) ;
#9964 = CARTESIAN_POINT ( 'NONE',  ( 2.789999999999999147, 15.04425356660760293, 20.70663861606276868 ) ) ;
#9965 = ORIENTED_EDGE ( 'NONE', *, *, #10073, .F. ) ;
#9966 = LINE ( 'NONE', #19151, #15307 ) ;
#9967 = CARTESIAN_POINT ( 'NONE',  ( 7.312499995903225525, -3.980288726281172656E-14, 5.700000000000001066 ) ) ;
#9968 = AXIS2_PLACEMENT_3D ( 'NONE', #7224, #11294, #14501 ) ;
#9969 = DIRECTION ( 'NONE',  ( -1.000000000000000000, 1.224646799147353207E-16, 0.000000000000000000 ) ) ;
#9970 = VERTEX_POINT ( 'NONE', #1076 ) ;
#9971 = AXIS2_PLACEMENT_3D ( 'NONE', #16547, #15042, #13537 ) ;
#9972 = EDGE_CURVE ( 'NONE', #3395, #9359, #16797, .T. ) ;
#9973 = ORIENTED_EDGE ( 'NONE', *, *, #8534, .F. ) ;
#9974 = TOROIDAL_SURFACE ( 'NONE', #3887, 24.12539914357697413, 8.000000000000000000 ) ;
#9975 = CIRCLE ( 'NONE', #13789, 5.400000000000000355 ) ;
#9976 = DIRECTION ( 'NONE',  ( -1.000000000000000000, -0.000000000000000000, -0.000000000000000000 ) ) ;
#9977 = CARTESIAN_POINT ( 'NONE',  ( 12.50000000000000533, -5.142044285764733935, -2.620002426024580000 ) ) ;
#9978 = ORIENTED_EDGE ( 'NONE', *, *, #9401, .F. ) ;
#9979 = CARTESIAN_POINT ( 'NONE',  ( 6.968749997951614539, -4.620319390059842490, 1.773574444220693103 ) ) ;
#9980 = CARTESIAN_POINT ( 'NONE',  ( 4.620319390059829168, 1.773574444220725299, -11.96874999795161365 ) ) ;
#9981 = EDGE_CURVE ( 'NONE', #6991, #17102, #13279, .T. ) ;
#9982 = VERTEX_POINT ( 'NONE', #2661 ) ;
#9983 = ORIENTED_EDGE ( 'NONE', *, *, #14341, .F. ) ;
#9984 = CARTESIAN_POINT ( 'NONE',  ( -5.207209108562852684, -2.318398865532001363, -8.000000000000005329 ) ) ;
#9985 = CARTESIAN_POINT ( 'NONE',  ( 13.00000000000000533, -5.207209108562836697, 2.318398865532038666 ) ) ;
#9986 = EDGE_CURVE ( 'NONE', #18451, #15630, #14881, .T. ) ;
#9987 = CIRCLE ( 'NONE', #3902, 40.00000000000000711 ) ;
#9988 = DIRECTION ( 'NONE',  ( 1.000000000000000000, 0.000000000000000000, 0.000000000000000000 ) ) ;
#9989 = VECTOR ( 'NONE', #19764, 1000.000000000000000 ) ;
#9990 = ORIENTED_EDGE ( 'NONE', *, *, #7510, .T. ) ;
#9991 = CARTESIAN_POINT ( 'NONE',  ( 11.96874999795161365, 3.114526743279308896, -3.846120219227901593 ) ) ;
#9992 = CIRCLE ( 'NONE', #3275, 0.1999999999999987899 ) ;
#9993 = CARTESIAN_POINT ( 'NONE',  ( 10.31249999590322552, -0.5958122406255588199, -5.668774803599165857 ) ) ;
#9994 = ORIENTED_EDGE ( 'NONE', *, *, #6103, .F. ) ;
#9995 = DIRECTION ( 'NONE',  ( 0.000000000000000000, 0.000000000000000000, 1.000000000000000000 ) ) ;
#9996 = VECTOR ( 'NONE', #19282, 1000.000000000000000 ) ;
#9997 = CARTESIAN_POINT ( 'NONE',  ( -19.00000000000000355, 3.278623949159157558, -2.625000000000002220 ) ) ;
#9998 = DIRECTION ( 'NONE',  ( 0.000000000000000000, 0.000000000000000000, 1.000000000000000000 ) ) ;
#9999 = DIRECTION ( 'NONE',  ( 1.000000000000000000, 0.000000000000000000, 0.000000000000000000 ) ) ;
#10000 = CARTESIAN_POINT ( 'NONE',  ( -12.32184790671639085, 13.12143529358541549, 32.00000000000000000 ) ) ;
#10001 = FILL_AREA_STYLE_COLOUR ( '', #4918 ) ;
#10002 = CARTESIAN_POINT ( 'NONE',  ( 0.000000000000000000, 20.70663861606293210, -15.04425356660737556 ) ) ;
#10003 = AXIS2_PLACEMENT_3D ( 'NONE', #7829, #9345, #11141 ) ;
#10004 =( NAMED_UNIT ( * ) PLANE_ANGLE_UNIT ( ) SI_UNIT ( $, .RADIAN. ) );
#10005 = ORIENTED_EDGE ( 'NONE', *, *, #9296, .T. ) ;
#10006 = EDGE_CURVE ( 'NONE', #4548, #11655, #498, .T. ) ;
#10007 = CARTESIAN_POINT ( 'NONE',  ( 12.31249999590322552, 2.849999999999989875, 4.936344801571308061 ) ) ;
#10008 = CARTESIAN_POINT ( 'NONE',  ( -41.99999999999999289, -2.000000000000001776, -5.000000000000000000 ) ) ;
#10009 = VECTOR ( 'NONE', #9348, 1000.000000000000114 ) ;
#10010 = PRODUCT_DEFINITION_CONTEXT ( 'detailed design', #884, 'design' ) ;
#10011 = CARTESIAN_POINT ( 'NONE',  ( 3.143139765844590983, -4.840010801796506890, -13.81249999590322552 ) ) ;
#10012 = VECTOR ( 'NONE', #8269, 1000.000000000000000 ) ;
#10013 = CARTESIAN_POINT ( 'NONE',  ( 16.96448111170888851, 1.130229351527639370, 32.00000000000000000 ) ) ;
#10014 = PLANE ( 'NONE',  #5497 ) ;
#10015 =( REPRESENTATION_RELATIONSHIP ('NONE','NONE', #18211, #2475 ) REPRESENTATION_RELATIONSHIP_WITH_TRANSFORMATION ( #14353 )SHAPE_REPRESENTATION_RELATIONSHIP( ) );
#10016 = CARTESIAN_POINT ( 'NONE',  ( -4.620319390059842490, -1.773574444220693325, -12.34374999795161543 ) ) ;
#10017 = EDGE_CURVE ( 'NONE', #11614, #1584, #948, .T. ) ;
#10018 = EDGE_LOOP ( 'NONE', ( #355, #10850 ) ) ;
#10019 = CARTESIAN_POINT ( 'NONE',  ( 13.34374999795161365, -4.409619785863891472, -2.246813503491864150 ) ) ;
#10020 = CARTESIAN_POINT ( 'NONE',  ( -9.000000000000000000, 1.102182119232617714E-15, 29.00000000000000355 ) ) ;
#10021 = TOROIDAL_SURFACE ( 'NONE', #16086, 24.12539914357697413, 8.000000000000000000 ) ;
#10022 = EDGE_LOOP ( 'NONE', ( #9799, #14259, #11079, #11564, #12666, #3512 ) ) ;
#10023 = CARTESIAN_POINT ( 'NONE',  ( -36.00000000000000000, -2.311115933264683024E-31, 0.000000000000000000 ) ) ;
#10024 = AXIS2_PLACEMENT_3D ( 'NONE', #17244, #18741, #240 ) ;
#10025 = AXIS2_PLACEMENT_3D ( 'NONE', #602, #5088, #11306 ) ;
#10026 = CARTESIAN_POINT ( 'NONE',  ( 1.039999999999995373, 25.12109765559670649, -12.52377138324197681 ) ) ;
#10027 = DIRECTION ( 'NONE',  ( -1.000000000000000000, -0.000000000000000000, -0.000000000000000000 ) ) ;
#10028 = EDGE_LOOP ( 'NONE', ( #12493, #8825, #13934, #14011 ) ) ;
#10029 = DIRECTION ( 'NONE',  ( 0.000000000000000000, 0.000000000000000000, 1.000000000000000000 ) ) ;
#10030 =( LENGTH_UNIT ( ) NAMED_UNIT ( * ) SI_UNIT ( .MILLI., .METRE. ) );
#10031 = DIRECTION ( 'NONE',  ( 1.000000000000000000, 0.000000000000000000, 0.000000000000000000 ) ) ;
#10032 = CARTESIAN_POINT ( 'NONE',  ( 1.255998204157470211, -17.85806462366060288, 35.00000000000000000 ) ) ;
#10033 = VERTEX_POINT ( 'NONE', #17657 ) ;
#10034 = DIRECTION ( 'NONE',  ( -1.000000000000000000, 0.000000000000000000, 0.000000000000000000 ) ) ;
#10035 = PRESENTATION_LAYER_ASSIGNMENT (  '', '', ( #9068 ) ) ;
#10036 = ORIENTED_EDGE ( 'NONE', *, *, #18513, .T. ) ;
#10037 = DIRECTION ( 'NONE',  ( 1.000000000000000000, 0.000000000000000000, 0.000000000000000000 ) ) ;
#10038 = CARTESIAN_POINT ( 'NONE',  ( 13.00000000000000178, -3.789407127742538517, 3.087705756618167374 ) ) ;
#10039 = PRODUCT_DEFINITION_SHAPE ( 'NONE', 'NONE',  #8091 ) ;
#10040 = FACE_OUTER_BOUND ( 'NONE', #4805, .T. ) ;
#10041 = FACE_OUTER_BOUND ( 'NONE', #7948, .T. ) ;
#10042 = EDGE_CURVE ( 'NONE', #1853, #12828, #2709, .T. ) ;
#10043 = ORIENTED_EDGE ( 'NONE', *, *, #8943, .T. ) ;
#10044 = CARTESIAN_POINT ( 'NONE',  ( -41.99999999999999289, 4.999999999999998224, 5.000000000000000000 ) ) ;
#10045 = SHAPE_REPRESENTATION ( 'DUST CUP', ( #16724 ), #3632 ) ;
#10046 = DIRECTION ( 'NONE',  ( 0.000000000000000000, 0.000000000000000000, 1.000000000000000000 ) ) ;
#10047 = ORIENTED_EDGE ( 'NONE', *, *, #11034, .F. ) ;
#10048 = CONICAL_SURFACE ( 'NONE', #3040, 3.889375000000000693, 0.9599310885968779239 ) ;
#10049 = DIRECTION ( 'NONE',  ( -0.000000000000000000, -0.000000000000000000, 1.000000000000000000 ) ) ;
#10050 = CARTESIAN_POINT ( 'NONE',  ( 0.5321745227542316048, 19.66801664102731095, -18.57583492944399950 ) ) ;
#10051 = ORIENTED_EDGE ( 'NONE', *, *, #16110, .F. ) ;
#10052 = DIRECTION ( 'NONE',  ( 0.000000000000000000, 0.000000000000000000, -1.000000000000000000 ) ) ;
#10053 = DIRECTION ( 'NONE',  ( -0.000000000000000000, -0.000000000000000000, 1.000000000000000000 ) ) ;
#10054 = FACE_BOUND ( 'NONE', #3833, .T. ) ;
#10055 = AXIS2_PLACEMENT_3D ( 'NONE', #15992, #2282, #6059 ) ;
#10056 = VERTEX_POINT ( 'NONE', #17751 ) ;
#10057 = ADVANCED_FACE ( 'NONE', ( #19152 ), #3848, .T. ) ;
#10058 = DIRECTION ( 'NONE',  ( 1.000000000000000000, 0.000000000000000000, 0.000000000000000000 ) ) ;
#10059 = ORIENTED_EDGE ( 'NONE', *, *, #3486, .F. ) ;
#10060 = CARTESIAN_POINT ( 'NONE',  ( 8.000000000000000000, 0.000000000000000000, 0.000000000000000000 ) ) ;
#10061 = CARTESIAN_POINT ( 'NONE',  ( -2.000000000000001776, 3.478305785123969152, -3.241971077674649315 ) ) ;
#10062 = ORIENTED_EDGE ( 'NONE', *, *, #6095, .T. ) ;
#10063 = CARTESIAN_POINT ( 'NONE',  ( 111.3234999999999957, 4.898587196589412829E-16, -4.000000000000000000 ) ) ;
#10064 = DIRECTION ( 'NONE',  ( -0.000000000000000000, -0.000000000000000000, 1.000000000000000000 ) ) ;
#10065 = EDGE_CURVE ( 'NONE', #11016, #18417, #11358, .T. ) ;
#10066 = AXIS2_PLACEMENT_3D ( 'NONE', #10269, #3962, #12973 ) ;
#10067 = DIRECTION ( 'NONE',  ( -1.000000000000000000, 1.224646799147353207E-16, 0.000000000000000000 ) ) ;
#10068 = VERTEX_POINT ( 'NONE', #11551 ) ;
#10069 = EDGE_CURVE ( 'NONE', #16569, #3939, #3948, .T. ) ;
#10070 = CARTESIAN_POINT ( 'NONE',  ( 2.299999999999998934, 0.000000000000000000, 0.000000000000000000 ) ) ;
#10071 = CIRCLE ( 'NONE', #12288, 9.000000000000000000 ) ;
#10072 = VERTEX_POINT ( 'NONE', #8645 ) ;
#10073 = EDGE_CURVE ( 'NONE', #3037, #18092, #18399, .T. ) ;
#10074 = CIRCLE ( 'NONE', #3990, 1.000000000000004441 ) ;
#10075 = CARTESIAN_POINT ( 'NONE',  ( 13.86923836996420789, -11.47363181547641453, 32.00000000000000000 ) ) ;
#10076 = LINE ( 'NONE', #8368, #10312 ) ;
#10077 = ORIENTED_EDGE ( 'NONE', *, *, #6483, .F. ) ;
#10078 = CARTESIAN_POINT ( 'NONE',  ( -4.620319390059805187, 1.773574444220790136, -11.34374999795161543 ) ) ;
#10079 =( LENGTH_UNIT ( ) NAMED_UNIT ( * ) SI_UNIT ( .MILLI., .METRE. ) );
#10080 = EDGE_CURVE ( 'NONE', #9454, #2779, #3481, .T. ) ;
#10081 = ORIENTED_EDGE ( 'NONE', *, *, #12844, .F. ) ;
#10082 = ORIENTED_EDGE ( 'NONE', *, *, #5985, .F. ) ;
#10083 = CARTESIAN_POINT ( 'NONE',  ( -4.465502636338051445, -1.988169868018530462, -8.468749997951615427 ) ) ;
#10084 = CARTESIAN_POINT ( 'NONE',  ( 13.46874999795161543, -4.465502636338038123, 1.988169868018562880 ) ) ;
#10085 = DIRECTION ( 'NONE',  ( -1.000000000000000000, -0.000000000000000000, -0.000000000000000000 ) ) ;
#10086 = DIRECTION ( 'NONE',  ( 0.000000000000000000, 0.000000000000000000, 1.000000000000000000 ) ) ;
#10087 = AXIS2_PLACEMENT_3D ( 'NONE', #5428, #2138, #11352 ) ;
#10088 = ORIENTED_EDGE ( 'NONE', *, *, #1272, .F. ) ;
#10089 = CARTESIAN_POINT ( 'NONE',  ( 0.02436607992776498519, -21.30679549418621832, -12.59161484032935618 ) ) ;
#10090 = CARTESIAN_POINT ( 'NONE',  ( 13.00000000000000533, -3.985098679772345331, 2.831373229855499662 ) ) ;
#10091 = ORIENTED_EDGE ( 'NONE', *, *, #6025, .T. ) ;
#10092 = CARTESIAN_POINT ( 'NONE',  ( 0.000000000000000000, 0.000000000000000000, -35.00000000000000000 ) ) ;
#10093 = EDGE_CURVE ( 'NONE', #14863, #3605, #12652, .T. ) ;
#10094 = DIRECTION ( 'NONE',  ( 0.000000000000000000, 0.000000000000000000, 1.000000000000000000 ) ) ;
#10095 = CARTESIAN_POINT ( 'NONE',  ( 4.366025403784385972, 7.562177826491085497, 41.99999999999999289 ) ) ;
#10096 = CARTESIAN_POINT ( 'NONE',  ( 7.343749997951615427, -4.620319390059842490, 1.773574444220693103 ) ) ;
#10097 = AXIS2_PLACEMENT_3D ( 'NONE', #4143, #5827, #12146 ) ;
#10098 = DIRECTION ( 'NONE',  ( -0.000000000000000000, -0.000000000000000000, 1.000000000000000000 ) ) ;
#10099 = CARTESIAN_POINT ( 'NONE',  ( 2.765633920072235963, 21.30679549418649543, -12.59161484032888723 ) ) ;
#10100 = AXIS2_PLACEMENT_3D ( 'NONE', #8969, #13569, #19669 ) ;
#10101 = EDGE_LOOP ( 'NONE', ( #13718, #2974, #148, #3654, #5065 ) ) ;
#10102 = CARTESIAN_POINT ( 'NONE',  ( 9.812499995903225525, 5.574407415329157622, 1.493657965219523875 ) ) ;
#10103 = DIRECTION ( 'NONE',  ( -0.000000000000000000, -0.000000000000000000, 1.000000000000000000 ) ) ;
#10104 = CARTESIAN_POINT ( 'NONE',  ( 5.763142191869155440, -0.3020334839682879413, -10.81249999590322375 ) ) ;
#10105 = FACE_OUTER_BOUND ( 'NONE', #9394, .T. ) ;
#10106 = CARTESIAN_POINT ( 'NONE',  ( -2.620002426024544473, 5.142044285764749922, -10.81249999590322375 ) ) ;
#10107 = ORIENTED_EDGE ( 'NONE', *, *, #13571, .T. ) ;
#10108 = CARTESIAN_POINT ( 'NONE',  ( 0.7589665089996491254, -24.80232951178369660, -12.05173163741749320 ) ) ;
#10109 = CARTESIAN_POINT ( 'NONE',  ( -11.32184790671638730, 13.12143529358541549, 32.00000000000000000 ) ) ;
#10110 = AXIS2_PLACEMENT_3D ( 'NONE', #13927, #220, #15529 ) ;
#10111 = EDGE_LOOP ( 'NONE', ( #12299, #6828, #12877, #19269 ) ) ;
#10112 = CARTESIAN_POINT ( 'NONE',  ( 2.789999999999999147, 9.324097380959765147, -22.25075486061728824 ) ) ;
#10113 = CIRCLE ( 'NONE', #7194, 8.265000000000021885 ) ;
#10114 = EDGE_CURVE ( 'NONE', #1346, #11278, #5799, .T. ) ;
#10115 = CARTESIAN_POINT ( 'NONE',  ( 1.749999999999998002, 4.633866840648922292, 27.68468304288260384 ) ) ;
#10116 = DIRECTION ( 'NONE',  ( 0.000000000000000000, 0.000000000000000000, 1.000000000000000000 ) ) ;
#10117 = CARTESIAN_POINT ( 'NONE',  ( 0.000000000000000000, 2.680914349914567470E-13, -25.59481291497571220 ) ) ;
#10118 = ORIENTED_EDGE ( 'NONE', *, *, #8356, .T. ) ;
#10119 = DIRECTION ( 'NONE',  ( 0.000000000000000000, 0.000000000000000000, -1.000000000000000000 ) ) ;
#10120 = DIRECTION ( 'NONE',  ( -1.000000000000000000, -0.000000000000000000, -0.000000000000000000 ) ) ;
#10121 = EDGE_CURVE ( 'NONE', #9330, #15039, #19347, .T. ) ;
#10122 = CARTESIAN_POINT ( 'NONE',  ( 0.000000000000000000, -7.909232158574988958, 24.34211360614297348 ) ) ;
#10123 = ORIENTED_EDGE ( 'NONE', *, *, #14313, .T. ) ;
#10124 = CARTESIAN_POINT ( 'NONE',  ( 11.81249999590322552, -3.631840208645763735, -4.484949146646406426 ) ) ;
#10125 = AXIS2_PLACEMENT_3D ( 'NONE', #5083, #5181, #18892 ) ;
#10126 = VERTEX_POINT ( 'NONE', #9774 ) ;
#10127 = CARTESIAN_POINT ( 'NONE',  ( 0.000000000000000000, 0.000000000000000000, 41.99999999999999289 ) ) ;
#10128 = AXIS2_PLACEMENT_3D ( 'NONE', #16998, #282, #187 ) ;
#10129 = CARTESIAN_POINT ( 'NONE',  ( 2.620002426024544029, 5.142044285764751699, -13.81249999590322730 ) ) ;
#10130 = CYLINDRICAL_SURFACE ( 'NONE', #1020, 6.000000000000021316 ) ;
#10131 = ADVANCED_FACE ( 'NONE', ( #8461 ), #14565, .T. ) ;
#10132 = DIRECTION ( 'NONE',  ( -0.000000000000000000, -0.000000000000000000, 1.000000000000000000 ) ) ;
#10133 = ORIENTED_EDGE ( 'NONE', *, *, #6340, .T. ) ;
#10134 = DIRECTION ( 'NONE',  ( 1.000000000000000000, 0.000000000000000000, 0.000000000000000000 ) ) ;
#10135 = DIRECTION ( 'NONE',  ( 0.000000000000000000, 0.000000000000000000, -1.000000000000000000 ) ) ;
#10136 = ORIENTED_EDGE ( 'NONE', *, *, #1855, .F. ) ;
#10137 = CIRCLE ( 'NONE', #2150, 2.524999999999997247 ) ;
#10138 = AXIS2_PLACEMENT_3D ( 'NONE', #14539, #2217, #8526 ) ;
#10139 = CARTESIAN_POINT ( 'NONE',  ( 2.255998204157473097, -17.85806462366060288, 32.00000000000000000 ) ) ;
#10140 = CARTESIAN_POINT ( 'NONE',  ( -4.080749450109677490, -4.080749450109621534, -14.81249999590322552 ) ) ;
#10141 = ORIENTED_EDGE ( 'NONE', *, *, #2136, .F. ) ;
#10142 = LINE ( 'NONE', #553, #14559 ) ;
#10143 = DIRECTION ( 'NONE',  ( 1.000000000000000000, 0.000000000000000000, 0.000000000000000000 ) ) ;
#10144 = CARTESIAN_POINT ( 'NONE',  ( 7.468749997951615427, 1.510506337161861445, -4.648860486681953397 ) ) ;
#10145 = ADVANCED_FACE ( 'NONE', ( #13057 ), #10644, .F. ) ;
#10146 = ORIENTED_EDGE ( 'NONE', *, *, #17983, .F. ) ;
#10147 = CARTESIAN_POINT ( 'NONE',  ( 2.789999999999999147, -14.55412442567631537, 19.64056340710869719 ) ) ;
#10148 = FACE_OUTER_BOUND ( 'NONE', #5659, .T. ) ;
#10149 = ORIENTED_EDGE ( 'NONE', *, *, #2944, .T. ) ;
#10150 = CARTESIAN_POINT ( 'NONE',  ( 12.86923836996420967, -11.47363181547641453, -32.00000000000000000 ) ) ;
#10151 = CARTESIAN_POINT ( 'NONE',  ( 2.789999999999999147, 25.59481291497571220, 0.000000000000000000 ) ) ;
#10152 = CARTESIAN_POINT ( 'NONE',  ( -2.500000000000002220, 0.000000000000000000, 0.000000000000000000 ) ) ;
#10153 = VERTEX_POINT ( 'NONE', #15044 ) ;
#10154 = DIRECTION ( 'NONE',  ( -0.000000000000000000, -0.000000000000000000, 1.000000000000000000 ) ) ;
#10155 = CARTESIAN_POINT ( 'NONE',  ( 6.000000000000005329, 4.936344801571289409, 2.850000000000024070 ) ) ;
#10156 = CIRCLE ( 'NONE', #15572, 22.00000000000000355 ) ;
#10157 = CARTESIAN_POINT ( 'NONE',  ( 0.02436607992776064838, 18.55949924794892780, 16.37294372382865504 ) ) ;
#10158 = AXIS2_PLACEMENT_3D ( 'NONE', #13436, #16454, #10356 ) ;
#10159 = ORIENTED_EDGE ( 'NONE', *, *, #6619, .F. ) ;
#10160 = CARTESIAN_POINT ( 'NONE',  ( -90.00000000000000000, 0.000000000000000000, -8.073750000000021743 ) ) ;
#10161 = ADVANCED_FACE ( 'NONE', ( #16749 ), #19190, .F. ) ;
#10162 = ORIENTED_EDGE ( 'NONE', *, *, #2158, .F. ) ;
#10163 = ADVANCED_FACE ( 'NONE', ( #19642 ), #4974, .T. ) ;
#10164 = CIRCLE ( 'NONE', #7259, 3.000000000000000000 ) ;
#10165 = CARTESIAN_POINT ( 'NONE',  ( 13.86923836996420789, -11.47363181547641453, -32.00000000000000000 ) ) ;
#10166 = VECTOR ( 'NONE', #4215, 1000.000000000000000 ) ;
#10167 = CARTESIAN_POINT ( 'NONE',  ( 2.789999999999999147, -22.25075486061731667, -9.324097380959683434 ) ) ;
#10168 = VERTEX_POINT ( 'NONE', #17848 ) ;
#10169 = CYLINDRICAL_SURFACE ( 'NONE', #18039, 1.000000000000002665 ) ;
#10170 = EDGE_CURVE ( 'NONE', #4088, #1239, #4019, .T. ) ;
#10171 = FILL_AREA_STYLE_COLOUR ( '', #11158 ) ;
#10172 = CARTESIAN_POINT ( 'NONE',  ( 0.8958345380406140812, -24.59696699259434993, 12.96989951879399250 ) ) ;
#10173 = ORIENTED_EDGE ( 'NONE', *, *, #14341, .T. ) ;
#10174 = ORIENTED_EDGE ( 'NONE', *, *, #7821, .F. ) ;
#10175 = LINE ( 'NONE', #16370, #6641 ) ;
#10176 = CARTESIAN_POINT ( 'NONE',  ( 7.500000000000005329, 3.143139765844590983, 4.840010801796506890 ) ) ;
#10177 = ORIENTED_EDGE ( 'NONE', *, *, #18687, .T. ) ;
#10178 = AXIS2_PLACEMENT_3D ( 'NONE', #7544, #18460, #19758 ) ;
#10179 = CARTESIAN_POINT ( 'NONE',  ( -9.671566133830877376, 15.77352024078954429, 32.00000000000000000 ) ) ;
#10180 = EDGE_LOOP ( 'NONE', ( #2210, #16284, #9365, #13956 ) ) ;
#10181 = CARTESIAN_POINT ( 'NONE',  ( -1.886022603841227552, 1.012170579495290078E-15, 8.265000000000021885 ) ) ;
#10182 = CARTESIAN_POINT ( 'NONE',  ( 10.84374999795161543, 1.016293382781477961, -4.781284448697179279 ) ) ;
#10183 = EDGE_LOOP ( 'NONE', ( #3414, #18475, #2555, #3644 ) ) ;
#10184 = DIRECTION ( 'NONE',  ( 1.000000000000000000, 0.000000000000000000, 0.000000000000000000 ) ) ;
#10185 = ADVANCED_FACE ( 'NONE', ( #1043 ), #10447, .T. ) ;
#10186 = CARTESIAN_POINT ( 'NONE',  ( 0.000000000000000000, 7.347880794884119736E-16, -6.000000000000000000 ) ) ;
#10187 = DIRECTION ( 'NONE',  ( -1.000000000000000000, 0.000000000000000000, -0.000000000000000000 ) ) ;
#10188 = CARTESIAN_POINT ( 'NONE',  ( 8.843749997951615427, -4.861323657744403448, -0.5109457054262123155 ) ) ;
#10189 = ADVANCED_FACE ( 'NONE', ( #16550 ), #14849, .F. ) ;
#10190 = PRODUCT_DEFINITION_SHAPE ( 'NONE', 'NONE',  #7325 ) ;
#10191 = ADVANCED_BREP_SHAPE_REPRESENTATION ( '', ( #16005, #16724 ), #2332 ) ;
#10192 = VECTOR ( 'NONE', #15612, 1000.000000000000000 ) ;
#10193 = CARTESIAN_POINT ( 'NONE',  ( 1.394999999999998685, -27.68468304288255410, -4.633866840649221608 ) ) ;
#10194 = CARTESIAN_POINT ( 'NONE',  ( -13.86923836996420967, -11.47363181547641275, 35.00000000000000000 ) ) ;
#10195 = ORIENTED_EDGE ( 'NONE', *, *, #15579, .F. ) ;
#10196 = DIRECTION ( 'NONE',  ( -0.000000000000000000, -0.000000000000000000, 1.000000000000000000 ) ) ;
#10197 = FACE_OUTER_BOUND ( 'NONE', #16017, .T. ) ;
#10198 = UNCERTAINTY_MEASURE_WITH_UNIT (LENGTH_MEASURE( 1.000000000000000082E-05 ), #7311, 'distance_accuracy_value', 'NONE');
#10199 = DIRECTION ( 'NONE',  ( 0.000000000000000000, 0.000000000000000000, -1.000000000000000000 ) ) ;
#10200 = PRODUCT_DEFINITION_FORMATION_WITH_SPECIFIED_SOURCE ( 'ANY', '', #17690, .NOT_KNOWN. ) ;
#10201 = EDGE_CURVE ( 'NONE', #14216, #1430, #17949, .T. ) ;
#10202 = LINE ( 'NONE', #7265, #18293 ) ;
#10203 = CARTESIAN_POINT ( 'NONE',  ( 4.611396867937200383, 3.350375938067097881, -15.31249999590322552 ) ) ;
#10204 = VERTEX_POINT ( 'NONE', #8942 ) ;
#10205 = CARTESIAN_POINT ( 'NONE',  ( -15.28688694438835505, -7.664027248171298545, -35.00000000000000000 ) ) ;
#10206 = DIRECTION ( 'NONE',  ( -1.000000000000000000, 0.000000000000000000, -0.000000000000000000 ) ) ;
#10207 = EDGE_CURVE ( 'NONE', #226, #257, #17757, .T. ) ;
#10208 = AXIS2_PLACEMENT_3D ( 'NONE', #6327, #18546, #1746 ) ;
#10209 = EDGE_LOOP ( 'NONE', ( #3749, #10931, #15656, #9554 ) ) ;
#10210 = CARTESIAN_POINT ( 'NONE',  ( 7.468749997951615427, -3.270778111535287191, -3.632567103900569361 ) ) ;
#10211 = ADVANCED_FACE ( 'NONE', ( #11035 ), #9143, .F. ) ;
#10212 = LINE ( 'NONE', #3707, #11219 ) ;
#10213 = AXIS2_PLACEMENT_3D ( 'NONE', #2244, #11457, #6832 ) ;
#10214 = DIRECTION ( 'NONE',  ( 1.000000000000000000, 0.000000000000000000, 0.000000000000000000 ) ) ;
#10215 = CARTESIAN_POINT ( 'NONE',  ( -4.611396867937224364, -3.350375938067065906, -15.31249999590322552 ) ) ;
#10216 = ORIENTED_EDGE ( 'NONE', *, *, #17176, .F. ) ;
#10217 = CARTESIAN_POINT ( 'NONE',  ( 1.039999999999997593, 0.000000000000000000, 0.000000000000000000 ) ) ;
#10218 = SHAPE_REPRESENTATION_RELATIONSHIP ( 'NONE' , 'NONE' ,  #15643, #10191 ) ;
#10219 = CARTESIAN_POINT ( 'NONE',  ( 2.718184757033982102, -18.89296398180179537, -16.91181672897754495 ) ) ;
#10220 = SURFACE_SIDE_STYLE ('',( #19501 ) ) ;
#10221 = ORIENTED_EDGE ( 'NONE', *, *, #12803, .F. ) ;
#10222 = LINE ( 'NONE', #19308, #5972 ) ;
#10223 = EDGE_LOOP ( 'NONE', ( #15818, #5941, #17066, #19284, #1916, #8397 ) ) ;
#10224 = UNCERTAINTY_MEASURE_WITH_UNIT (LENGTH_MEASURE( 1.000000000000000082E-05 ), #13882, 'distance_accuracy_value', 'NONE');
#10225 = LINE ( 'NONE', #5219, #4789 ) ;
#10226 = CARTESIAN_POINT ( 'NONE',  ( 2.765633920072242180, 22.71065055754465689, -9.836394144775473691 ) ) ;
#10227 = ADVANCED_FACE ( 'NONE', ( #5025 ), #11135, .F. ) ;
#10228 = DIRECTION ( 'NONE',  ( 1.000000000000000000, 0.000000000000000000, 0.000000000000000000 ) ) ;
#10229 = AXIS2_PLACEMENT_3D ( 'NONE', #12116, #4309, #11814 ) ;
#10230 = CARTESIAN_POINT ( 'NONE',  ( -18.68117051311639543, -3.372863662543042818, 35.00000000000000000 ) ) ;
#10231 = ORIENTED_EDGE ( 'NONE', *, *, #17245, .F. ) ;
#10232 = CARTESIAN_POINT ( 'NONE',  ( -4.465502636338010589, 1.988169868018623720, -14.84374999795161543 ) ) ;
#10233 = CARTESIAN_POINT ( 'NONE',  ( 2.999999999999998224, -3.218695387886215009, -3.000000000000001776 ) ) ;
#10234 = EDGE_CURVE ( 'NONE', #8854, #1430, #832, .T. ) ;
#10235 = ORIENTED_EDGE ( 'NONE', *, *, #12144, .T. ) ;
#10236 = EDGE_CURVE ( 'NONE', #13685, #19526, #4123, .T. ) ;
#10237 = FACE_BOUND ( 'NONE', #5695, .T. ) ;
#10238 = CARTESIAN_POINT ( 'NONE',  ( 4.409619785863891472, -2.246813503491864150, -8.343749997951611874 ) ) ;
#10239 = VERTEX_POINT ( 'NONE', #3227 ) ;
#10241 = CARTESIAN_POINT ( 'NONE',  ( -1.016293382781411125, 4.781284448697194378, -7.843749997951614539 ) ) ;
#10240 = CIRCLE ( 'NONE', #18540, 3.000000000000000000 ) ;
#10242 = EDGE_CURVE ( 'NONE', #8773, #13907, #9136, .T. ) ;
#10243 = FACE_OUTER_BOUND ( 'NONE', #7841, .T. ) ;
#10244 = AXIS2_PLACEMENT_3D ( 'NONE', #2818, #14840, #1134 ) ;
#10245 = CARTESIAN_POINT ( 'NONE',  ( 11.34374999795161543, -1.773574444220757496, 4.620319390059819398 ) ) ;
#10246 = ORIENTED_EDGE ( 'NONE', *, *, #3830, .F. ) ;
#10247 = PLANE ( 'NONE',  #12466 ) ;
#10248 = ORIENTED_EDGE ( 'NONE', *, *, #15781, .T. ) ;
#10249 = DIRECTION ( 'NONE',  ( 0.000000000000000000, 0.000000000000000000, 1.000000000000000000 ) ) ;
#10250 = ORIENTED_EDGE ( 'NONE', *, *, #12772, .F. ) ;
#10251 = CARTESIAN_POINT ( 'NONE',  ( 7.468749997951615427, 3.270778111535313837, 3.632567103900546712 ) ) ;
#10252 = CARTESIAN_POINT ( 'NONE',  ( -34.92499999999994742, 0.000000000000000000, 0.000000000000000000 ) ) ;
#10253 = FACE_OUTER_BOUND ( 'NONE', #2336, .T. ) ;
#10254 = DIRECTION ( 'NONE',  ( -1.000000000000000000, -1.224646799147353207E-16, 0.000000000000000000 ) ) ;
#10255 = CARTESIAN_POINT ( 'NONE',  ( 8.468749997951615427, -4.861323657744403448, -0.5109457054262123155 ) ) ;
#10256 = DIRECTION ( 'NONE',  ( 0.000000000000000000, 1.000000000000000000, 0.000000000000000000 ) ) ;
#10257 = EDGE_LOOP ( 'NONE', ( #6646, #16116, #15320, #10998 ) ) ;
#10258 = VECTOR ( 'NONE', #11801, 1000.000000000000114 ) ;
#10259 = PRESENTATION_LAYER_ASSIGNMENT (  '', '', ( #18875 ) ) ;
#10260 = EDGE_CURVE ( 'NONE', #16376, #9486, #10735, .T. ) ;
#10261 =( NAMED_UNIT ( * ) SI_UNIT ( $, .STERADIAN. ) SOLID_ANGLE_UNIT ( ) );
#10262 = EDGE_LOOP ( 'NONE', ( #10367, #11341, #16962, #1432, #14463, #5217, #14391 ) ) ;
#10263 = DIRECTION ( 'NONE',  ( -1.000000000000000000, -0.000000000000000000, -0.000000000000000000 ) ) ;
#10264 = DIRECTION ( 'NONE',  ( -1.000000000000000000, 0.000000000000000000, 0.000000000000000000 ) ) ;
#10265 = CARTESIAN_POINT ( 'NONE',  ( 5.566640002541124371E-16, 15.96500990068152426, -18.34424029220094354 ) ) ;
#10266 = CARTESIAN_POINT ( 'NONE',  ( 2.262072637928883800, -23.73240184472485836, -12.96450951081243375 ) ) ;
#10267 = ORIENTED_EDGE ( 'NONE', *, *, #13340, .T. ) ;
#10268 =( BOUNDED_SURFACE ( )  B_SPLINE_SURFACE ( 1, 2, ( 
 ( #231, #6314, #17042, #14034, #328, #4253, #16657, #2740, #5841, #12258, #3145, #6137, #15263, #13553, #1350, #4449, #18063 ),
 ( #1550, #7534, #13351, #18258, #7639, #19547, #15057, #10659, #13446, #4545, #10365, #7430, #19656, #2842, #13654, #19749, #4646 ) ),
 .UNSPECIFIED., .F., .F., .F. ) 
 B_SPLINE_SURFACE_WITH_KNOTS ( ( 2, 2 ),
 ( 3, 2, 2, 2, 2, 2, 2, 2, 3 ),
 ( 0.000000000000000000, 1.000000000000000000 ),
 ( 0.000000000000000000, 0.05000000000000000278, 0.1000000000000000056, 0.1499999999999999944, 0.2000000000000000111, 0.2500000000000000000, 0.2999999999999999889, 0.3499999999999999778, 0.4000000000000000222 ),
 .UNSPECIFIED. ) 
 GEOMETRIC_REPRESENTATION_ITEM ( )  RATIONAL_B_SPLINE_SURFACE ( (
 ( 1.000000000000000000, 0.9876883405951377704, 1.000000000000000000, 0.9876883405951377704, 1.000000000000000000, 0.9876883405951377704, 1.000000000000000000, 0.9876883405951377704, 1.000000000000000000, 0.9876883405951377704, 1.000000000000000000, 0.9876883405951377704, 1.000000000000000000, 0.9876883405951377704, 1.000000000000000000, 0.9876883405951377704, 1.000000000000000000),
 ( 1.000000000000000000, 0.9876883405951377704, 1.000000000000000000, 0.9876883405951377704, 1.000000000000000000, 0.9876883405951377704, 1.000000000000000000, 0.9876883405951377704, 1.000000000000000000, 0.9876883405951377704, 1.000000000000000000, 0.9876883405951377704, 1.000000000000000000, 0.9876883405951377704, 1.000000000000000000, 0.9876883405951377704, 1.000000000000000000) ) ) 
 REPRESENTATION_ITEM ( '' )  SURFACE ( )  );
#10269 = CARTESIAN_POINT ( 'NONE',  ( 12.32184790671639618, 13.12143529358541016, 32.00000000000000000 ) ) ;
#10270 = AXIS2_PLACEMENT_3D ( 'NONE', #1154, #4349, #5735 ) ;
#10271 = DIRECTION ( 'NONE',  ( -8.326672684688818267E-17, -1.998922689279512092E-30, 1.000000000000000000 ) ) ;
#10272 = DIRECTION ( 'NONE',  ( 0.000000000000000000, 0.000000000000000000, 1.000000000000000000 ) ) ;
#10273 = ORIENTED_EDGE ( 'NONE', *, *, #5632, .F. ) ;
#10274 = ADVANCED_FACE ( 'NONE', ( #8017 ), #7835, .T. ) ;
#10275 = ORIENTED_EDGE ( 'NONE', *, *, #1594, .F. ) ;
#10276 = CARTESIAN_POINT ( 'NONE',  ( 2.459751808031945922E-16, 12.51294990530016271, 20.85230829256858343 ) ) ;
#10277 = CARTESIAN_POINT ( 'NONE',  ( -2.849999999999989431, 4.936344801571308061, -7.312499995903225525 ) ) ;
#10278 = ORIENTED_EDGE ( 'NONE', *, *, #7251, .F. ) ;
#10279 = CARTESIAN_POINT ( 'NONE',  ( -1.800000000000000044, 0.000000000000000000, -7.800000000000000711 ) ) ;
#10280 = ORIENTED_EDGE ( 'NONE', *, *, #12220, .T. ) ;
#10281 = ADVANCED_FACE ( 'NONE', ( #18632 ), #15542, .F. ) ;
#10282 = ADVANCED_FACE ( 'NONE', ( #4931 ), #5604, .T. ) ;
#10283 = CARTESIAN_POINT ( 'NONE',  ( -41.99999999999999289, 1.999999999999998224, 2.000000000000000000 ) ) ;
#10284 = DIRECTION ( 'NONE',  ( 0.000000000000000000, 0.000000000000000000, 1.000000000000000000 ) ) ;
#10285 = AXIS2_PLACEMENT_3D ( 'NONE', #3115, #7504, #6203 ) ;
#10286 = ORIENTED_EDGE ( 'NONE', *, *, #15814, .F. ) ;
#10287 = CARTESIAN_POINT ( 'NONE',  ( 2.255998204157473097, -17.85806462366060288, -32.00000000000000000 ) ) ;
#10288 = CIRCLE ( 'NONE', #8688, 4.824999999999999289 ) ;
#10289 = DIRECTION ( 'NONE',  ( 1.000000000000000000, 0.000000000000000000, 0.000000000000000000 ) ) ;
#10290 = DIRECTION ( 'NONE',  ( 0.000000000000000000, 0.000000000000000000, -1.000000000000000000 ) ) ;
#10291 = CARTESIAN_POINT ( 'NONE',  ( 1.749999999999998002, -27.68468304288262516, 4.633866840648810381 ) ) ;
#10292 = LINE ( 'NONE', #14889, #9497 ) ;
#10293 = CYLINDRICAL_SURFACE ( 'NONE', #18604, 13.20000000000000284 ) ;
#10294 = VERTEX_POINT ( 'NONE', #6121 ) ;
#10295 = DIRECTION ( 'NONE',  ( 0.000000000000000000, 0.000000000000000000, -1.000000000000000000 ) ) ;
#10296 = VECTOR ( 'NONE', #5374, 1000.000000000000000 ) ;
#10297 = CARTESIAN_POINT ( 'NONE',  ( -15.00000000000000355, -5.400000000000000355, 0.000000000000000000 ) ) ;
#10298 = CIRCLE ( 'NONE', #19546, 1.000000000000003553 ) ;
#10299 = CARTESIAN_POINT ( 'NONE',  ( -1.799999999999999600, 0.000000000000000000, 0.000000000000000000 ) ) ;
#10300 = AXIS2_PLACEMENT_3D ( 'NONE', #17534, #11918, #5903 ) ;
#10301 = DIRECTION ( 'NONE',  ( 1.000000000000000000, 0.000000000000000000, 0.000000000000000000 ) ) ;
#10302 = LINE ( 'NONE', #16401, #13052 ) ;
#10303 = ORIENTED_EDGE ( 'NONE', *, *, #4073, .T. ) ;
#10304 = EDGE_CURVE ( 'NONE', #9647, #14916, #12967, .T. ) ;
#10305 = DIRECTION ( 'NONE',  ( 1.000000000000000000, 0.000000000000000000, -0.000000000000000000 ) ) ;
#10306 = AXIS2_PLACEMENT_3D ( 'NONE', #1383, #2870, #15184 ) ;
#10307 = ADVANCED_FACE ( 'NONE', ( #6216 ), #1829, .F. ) ;
#10308 = CARTESIAN_POINT ( 'NONE',  ( 17.11901729331276556, 5.562305898749055011, 32.00000000000000000 ) ) ;
#10309 = ORIENTED_EDGE ( 'NONE', *, *, #12794, .F. ) ;
#10310 = CARTESIAN_POINT ( 'NONE',  ( 13.81249999590322552, -4.840010801796506890, 3.143139765844590983 ) ) ;
#10311 = CARTESIAN_POINT ( 'NONE',  ( 11.81249999590322552, -3.631840208645764179, -4.484949146646406426 ) ) ;
#10312 = VECTOR ( 'NONE', #5356, 1000.000000000000000 ) ;
#10313 = PRESENTATION_LAYER_ASSIGNMENT (  '', '', ( #18930 ) ) ;
#10314 = CIRCLE ( 'NONE', #1684, 4.762500000000000178 ) ;
#10315 = CARTESIAN_POINT ( 'NONE',  ( -1.800000000000000488, 0.000000000000000000, 0.000000000000000000 ) ) ;
#10316 = CARTESIAN_POINT ( 'NONE',  ( 2.789999999999999147, 15.04425356660790136, -20.70663861606255196 ) ) ;
#10317 = ADVANCED_FACE ( 'NONE', ( #16850 ), #10268, .T. ) ;
#10318 = VERTEX_POINT ( 'NONE', #13754 ) ;
#10319 = CARTESIAN_POINT ( 'NONE',  ( 1.999999999999998668, -8.000000000000003553, 37.99999999999999289 ) ) ;
#10320 = CARTESIAN_POINT ( 'NONE',  ( 4.620319390059819398, -1.773574444220757496, -11.34374999795161543 ) ) ;
#10321 = CARTESIAN_POINT ( 'NONE',  ( 12.00000000000000355, 4.898587196589412829E-16, 4.000000000000000000 ) ) ;
#10322 = ORIENTED_EDGE ( 'NONE', *, *, #7570, .T. ) ;
#10323 = ADVANCED_FACE ( 'NONE', ( #16465 ), #11852, .F. ) ;
#10324 = LINE ( 'NONE', #19706, #2156 ) ;
#10325 = ORIENTED_EDGE ( 'NONE', *, *, #15785, .T. ) ;
#10327 = EDGE_CURVE ( 'NONE', #16968, #2987, #16767, .T. ) ;
#10326 = EDGE_CURVE ( 'NONE', #19705, #1381, #2103, .T. ) ;
#10328 = CARTESIAN_POINT ( 'NONE',  ( 8.776855558857221240, 3.635492607468361559, 12.00000000000000000 ) ) ;
#10329 = CARTESIAN_POINT ( 'NONE',  ( 11.34374999795161543, 4.888101187500000222, -0.7741991708318890497 ) ) ;
#10330 = CYLINDRICAL_SURFACE ( 'NONE', #6763, 6.735000000000022524 ) ;
#10331 = TOROIDAL_SURFACE ( 'NONE', #11901, 24.12539914357697768, 8.000000000000000000 ) ;
#10332 = DIRECTION ( 'NONE',  ( 0.000000000000000000, 0.000000000000000000, -1.000000000000000000 ) ) ;
#10333 = ORIENTED_EDGE ( 'NONE', *, *, #11485, .T. ) ;
#10334 = FACE_OUTER_BOUND ( 'NONE', #11084, .T. ) ;
#10335 = DIRECTION ( 'NONE',  ( 1.000000000000000000, 0.000000000000000000, 0.000000000000000000 ) ) ;
#10336 = ORIENTED_EDGE ( 'NONE', *, *, #8851, .T. ) ;
#10337 = AXIS2_PLACEMENT_3D ( 'NONE', #18941, #11350, #12747 ) ;
#10338 = AXIS2_PLACEMENT_3D ( 'NONE', #16343, #12115, #16824 ) ;
#10339 = DIRECTION ( 'NONE',  ( 0.000000000000000000, 0.000000000000000000, 1.000000000000000000 ) ) ;
#10340 = CARTESIAN_POINT ( 'NONE',  ( 1.039999999999996927, 20.02152543075374069, -19.67366047555508501 ) ) ;
#10341 = ORIENTED_EDGE ( 'NONE', *, *, #11919, .T. ) ;
#10342 = AXIS2_PLACEMENT_3D ( 'NONE', #14763, #12060, #16566 ) ;
#10343 = CARTESIAN_POINT ( 'NONE',  ( -0.2590123213420971182, 4.942249507334556924, -8.343749997951611874 ) ) ;
#10344 = CARTESIAN_POINT ( 'NONE',  ( 0.000000000000000000, 0.000000000000000000, -32.00000000000000000 ) ) ;
#10345 = FACE_BOUND ( 'NONE', #14518, .T. ) ;
#10346 = EDGE_LOOP ( 'NONE', ( #5500, #8970, #3738, #14924 ) ) ;
#10347 = CARTESIAN_POINT ( 'NONE',  ( 2.789999999999999147, -8.936381166381891568E-14, 25.59481291497571220 ) ) ;
#10348 = VERTEX_POINT ( 'NONE', #12158 ) ;
#10349 = CARTESIAN_POINT ( 'NONE',  ( -30.00000000000000000, -1.925929944387235853E-31, 0.000000000000000000 ) ) ;
#10350 = EDGE_LOOP ( 'NONE', ( #12269, #9825, #16083, #12175 ) ) ;
#10351 = DIRECTION ( 'NONE',  ( 1.000000000000000000, 0.000000000000000000, -0.000000000000000000 ) ) ;
#10352 = AXIS2_PLACEMENT_3D ( 'NONE', #8187, #18790, #18689 ) ;
#10353 = LINE ( 'NONE', #8940, #13154 ) ;
#10354 = CARTESIAN_POINT ( 'NONE',  ( 0.000000000000000000, 0.000000000000000000, -6.502399999999998847 ) ) ;
#10355 = CARTESIAN_POINT ( 'NONE',  ( 11.00000000000000711, -2.849999999999954792, -4.936344801571327601 ) ) ;
#10356 = DIRECTION ( 'NONE',  ( 1.000000000000000000, 0.000000000000000000, 0.000000000000000000 ) ) ;
#10357 = ORIENTED_EDGE ( 'NONE', *, *, #2835, .T. ) ;
#10358 = COLOUR_RGB ( '', 0.66274510, 0.83137255, 0.94901961) ;
#10359 = CARTESIAN_POINT ( 'NONE',  ( 1.749999999999998002, -19.67366047555515252, -20.02152543075368030 ) ) ;
#10360 = PRODUCT_DEFINITION_SHAPE ( 'NONE', 'NONE',  #19786 ) ;
#10361 = EDGE_LOOP ( 'NONE', ( #1172, #17917 ) ) ;
#10362 = VECTOR ( 'NONE', #7614, 1000.000000000000000 ) ;
#10363 = PLANE ( 'NONE',  #14423 ) ;
#10364 = LINE ( 'NONE', #7533, #4818 ) ;
#10365 = CARTESIAN_POINT ( 'NONE',  ( 4.936344801571289409, -2.850000000000023626, -11.00000000000000711 ) ) ;
#10366 = LINE ( 'NONE', #19657, #13848 ) ;
#10367 = ORIENTED_EDGE ( 'NONE', *, *, #9192, .F. ) ;
#10368 = CARTESIAN_POINT ( 'NONE',  ( 0.02436607992776585255, -5.391175441198789109, 24.15498966839961170 ) ) ;
#10369 = AXIS2_PLACEMENT_3D ( 'NONE', #14066, #473, #12579 ) ;
#10370 = ORIENTED_EDGE ( 'NONE', *, *, #14952, .F. ) ;
#10371 = APPLICATION_PROTOCOL_DEFINITION ( 'draft international standard', 'automotive_design', 1998, #2652 ) ;
#10372 = CARTESIAN_POINT ( 'NONE',  ( -4.620319390059841602, -1.773574444220693325, -11.96874999795161365 ) ) ;
#10373 = ADVANCED_FACE ( 'NONE', ( #11956 ), #16813, .T. ) ;
#10374 = ORIENTED_EDGE ( 'NONE', *, *, #12536, .F. ) ;
#10375 = EDGE_LOOP ( 'NONE', ( #19132, #16834, #17237, #15660 ) ) ;
#10376 = CARTESIAN_POINT ( 'NONE',  ( 1.999999999999999112, 5.143516556418882928E-16, 4.200000000000000178 ) ) ;
#10377 = DIRECTION ( 'NONE',  ( 0.000000000000000000, 0.000000000000000000, -1.000000000000000000 ) ) ;
#10379 = VERTEX_POINT ( 'NONE', #10558 ) ;
#10378 = TOROIDAL_SURFACE ( 'NONE', #1742, 24.12539914357697413, 8.000000000000000000 ) ;
#10380 = CARTESIAN_POINT ( 'NONE',  ( 0.7589665349472695111, -27.14933624560910630, 4.828387785247921116 ) ) ;
#10381 = ORIENTED_EDGE ( 'NONE', *, *, #979, .T. ) ;
#10382 = CARTESIAN_POINT ( 'NONE',  ( -10.00000000000000000, 0.000000000000000000, 0.000000000000000000 ) ) ;
#10383 = FACE_OUTER_BOUND ( 'NONE', #6268, .T. ) ;
#10384 = ORIENTED_EDGE ( 'NONE', *, *, #9793, .F. ) ;
#10385 = CARTESIAN_POINT ( 'NONE',  ( -20.63749999999999574, 9.797174393178825657E-16, 8.000000000000000000 ) ) ;
#10386 = EDGE_CURVE ( 'NONE', #8767, #3180, #4662, .T. ) ;
#10387 =( BOUNDED_SURFACE ( )  B_SPLINE_SURFACE ( 1, 2, ( 
 ( #7098, #4615, #17215, #11012, #12222, #7, #6100, #13918, #10721, #9318, #18323, #7900, #407, #6488, #12518, #12619, #213 ),
 ( #16832, #18515, #3110, #16927, #18705, #13816, #15326, #1611, #9222, #14015, #1809, #7701, #5006, #3506, #15617, #3206, #14110 ) ),
 .UNSPECIFIED., .F., .F., .F. ) 
 B_SPLINE_SURFACE_WITH_KNOTS ( ( 2, 2 ),
 ( 3, 2, 2, 2, 2, 2, 2, 2, 3 ),
 ( 0.000000000000000000, 1.000000000000000000 ),
 ( 0.000000000000000000, 0.05000000000000000278, 0.1000000000000000056, 0.1499999999999999944, 0.2000000000000000111, 0.2500000000000000000, 0.2999999999999999889, 0.3499999999999999778, 0.4000000000000000222 ),
 .UNSPECIFIED. ) 
 GEOMETRIC_REPRESENTATION_ITEM ( )  RATIONAL_B_SPLINE_SURFACE ( (
 ( 1.000000000000000000, 0.9876883405951377704, 1.000000000000000000, 0.9876883405951377704, 1.000000000000000000, 0.9876883405951377704, 1.000000000000000000, 0.9876883405951377704, 1.000000000000000000, 0.9876883405951377704, 1.000000000000000000, 0.9876883405951377704, 1.000000000000000000, 0.9876883405951377704, 1.000000000000000000, 0.9876883405951377704, 1.000000000000000000),
 ( 1.000000000000000000, 0.9876883405951377704, 1.000000000000000000, 0.9876883405951377704, 1.000000000000000000, 0.9876883405951377704, 1.000000000000000000, 0.9876883405951377704, 1.000000000000000000, 0.9876883405951377704, 1.000000000000000000, 0.9876883405951377704, 1.000000000000000000, 0.9876883405951377704, 1.000000000000000000, 0.9876883405951377704, 1.000000000000000000) ) ) 
 REPRESENTATION_ITEM ( '' )  SURFACE ( )  );
#10388 = VECTOR ( 'NONE', #4402, 1000.000000000000000 ) ;
#10389 = CARTESIAN_POINT ( 'NONE',  ( -36.00000000000000000, 1.224646799147351975E-16, 0.000000000000000000 ) ) ;
#10390 = CARTESIAN_POINT ( 'NONE',  ( 8.843749997951615427, 2.873153789725825469, -3.954556930911862000 ) ) ;
#10391 = DIRECTION ( 'NONE',  ( 0.000000000000000000, 0.000000000000000000, -1.000000000000000000 ) ) ;
#10392 = DIRECTION ( 'NONE',  ( 0.000000000000000000, 0.000000000000000000, 1.000000000000000000 ) ) ;
#10393 = CARTESIAN_POINT ( 'NONE',  ( 2.000000000000000000, 4.999999999999998224, 37.99999999999999289 ) ) ;
#10394 = ADVANCED_FACE ( 'NONE', ( #4353 ), #16564, .T. ) ;
#10395 = VERTEX_POINT ( 'NONE', #9156 ) ;
#10396 = DIRECTION ( 'NONE',  ( -1.000000000000000000, 0.000000000000000000, 0.000000000000000000 ) ) ;
#10397 = VECTOR ( 'NONE', #1692, 1000.000000000000114 ) ;
#10398 = DIRECTION ( 'NONE',  ( -1.000000000000000000, 0.000000000000000000, -0.000000000000000000 ) ) ;
#10399 = UNCERTAINTY_MEASURE_WITH_UNIT (LENGTH_MEASURE( 1.000000000000000082E-05 ), #8268, 'distance_accuracy_value', 'NONE');
#10400 = CYLINDRICAL_SURFACE ( 'NONE', #3851, 2.524999999999995914 ) ;
#10401 = DIRECTION ( 'NONE',  ( -1.000000000000000000, -0.000000000000000000, -0.000000000000000000 ) ) ;
#10402 = CARTESIAN_POINT ( 'NONE',  ( 12.99999999999999467, 4.521642095224343905, 1.858077407906634892 ) ) ;
#10403 = ORIENTED_EDGE ( 'NONE', *, *, #1023, .T. ) ;
#10404 = DIRECTION ( 'NONE',  ( 0.000000000000000000, 0.000000000000000000, 1.000000000000000000 ) ) ;
#10405 = ORIENTED_EDGE ( 'NONE', *, *, #6016, .F. ) ;
#10406 = CARTESIAN_POINT ( 'NONE',  ( 12.32184790671639618, 13.12143529358541016, -35.00000000000000000 ) ) ;
#10407 = EDGE_CURVE ( 'NONE', #8838, #12604, #6244, .T. ) ;
#10408 = CARTESIAN_POINT ( 'NONE',  ( 14.81249999590322552, 1.493657965219562067, -5.574407415329146964 ) ) ;
#10409 = AXIS2_PLACEMENT_3D ( 'NONE', #18450, #6229, #15652 ) ;
#10410 = CARTESIAN_POINT ( 'NONE',  ( 2.031033471609898111, -27.31260702007178409, 3.797536611356223890 ) ) ;
#10411 = DIRECTION ( 'NONE',  ( -1.000000000000000000, -0.000000000000000000, -0.000000000000000000 ) ) ;
#10412 = ADVANCED_FACE ( 'NONE', ( #1452 ), #8173, .T. ) ;
#10413 = ORIENTED_EDGE ( 'NONE', *, *, #6129, .T. ) ;
#10414 = CARTESIAN_POINT ( 'NONE',  ( 7.968749997951616315, 2.246813503491833508, -4.409619785863906571 ) ) ;
#10415 = FILL_AREA_STYLE ('',( #7282 ) ) ;
#10416 = ORIENTED_EDGE ( 'NONE', *, *, #18151, .F. ) ;
#10417 = EDGE_CURVE ( 'NONE', #1763, #12919, #2722, .T. ) ;
#10418 = CARTESIAN_POINT ( 'NONE',  ( 0.000000000000000000, -15.04425356660744839, -20.70663861606288236 ) ) ;
#10419 = ORIENTED_EDGE ( 'NONE', *, *, #5009, .T. ) ;
#10420 = B_SPLINE_CURVE_WITH_KNOTS ( 'NONE', 3,
 ( #12850, #5338, #7113, #13142, #17553, #751 ),
 .UNSPECIFIED., .F., .F.,
 ( 4, 2, 4 ),
 ( 2.321268216996885854E-07, 0.001878622960950492504, 0.003757013795079285415 ),
 .UNSPECIFIED. ) ;
#10421 = CYLINDRICAL_SURFACE ( 'NONE', #14723, 5.700000000000001954 ) ;
#10422 = CARTESIAN_POINT ( 'NONE',  ( 13.46874999795161543, 3.954556930911862000, 2.873153789725825025 ) ) ;
#10423 = CARTESIAN_POINT ( 'NONE',  ( 13.00000000000000533, 0.5958122406256767256, -5.668774803599153422 ) ) ;
#10424 = AXIS2_PLACEMENT_3D ( 'NONE', #13138, #16242, #8341 ) ;
#10425 = CARTESIAN_POINT ( 'NONE',  ( 4.861323657744407001, -0.5109457054261775655, -13.84374999795161543 ) ) ;
#10426 = ORIENTED_EDGE ( 'NONE', *, *, #1255, .T. ) ;
#10427 = CARTESIAN_POINT ( 'NONE',  ( -4.942249507334558700, -0.2590123213420631454, -13.34374999795161365 ) ) ;
#10428 = EDGE_CURVE ( 'NONE', #3802, #11052, #16478, .T. ) ;
#10429 = DIRECTION ( 'NONE',  ( -0.000000000000000000, 0.000000000000000000, 1.000000000000000000 ) ) ;
#10430 = EDGE_LOOP ( 'NONE', ( #16342, #7004, #1672, #9657 ) ) ;
#10431 = EDGE_CURVE ( 'NONE', #12806, #5646, #18745, .T. ) ;
#10432 = EDGE_CURVE ( 'NONE', #7032, #6786, #9457, .T. ) ;
#10433 = CARTESIAN_POINT ( 'NONE',  ( -2.246813503491833508, 4.409619785863906571, -10.34374999795161543 ) ) ;
#10434 = CARTESIAN_POINT ( 'NONE',  ( 2.262072661820536013, 26.82026385750178932, -3.461047254864356049 ) ) ;
#10435 = ORIENTED_EDGE ( 'NONE', *, *, #10749, .F. ) ;
#10436 = CIRCLE ( 'NONE', #4688, 4.400000000000000355 ) ;
#10437 = CARTESIAN_POINT ( 'NONE',  ( 4.465502636338025688, -1.988169868018592856, -14.46874999795161720 ) ) ;
#10438 = DIRECTION ( 'NONE',  ( -1.000000000000000000, 0.000000000000000000, 0.000000000000000000 ) ) ;
#10439 = DIRECTION ( 'NONE',  ( -1.000000000000000000, -0.000000000000000000, 0.000000000000000000 ) ) ;
#10440 = ORIENTED_EDGE ( 'NONE', *, *, #11247, .T. ) ;
#10441 = DIRECTION ( 'NONE',  ( 0.000000000000000000, 0.000000000000000000, 1.000000000000000000 ) ) ;
#10442 = ORIENTED_EDGE ( 'NONE', *, *, #3994, .F. ) ;
#10443 = DIRECTION ( 'NONE',  ( 6.982962677686267499E-15, 1.000000000000000000, -0.000000000000000000 ) ) ;
#10444 = ORIENTED_EDGE ( 'NONE', *, *, #12443, .F. ) ;
#10445 = CARTESIAN_POINT ( 'NONE',  ( -14.00000000000000178, 0.000000000000000000, -32.00000000000000000 ) ) ;
#10446 = CARTESIAN_POINT ( 'NONE',  ( 13.00000000000000178, 4.568735188514060575, 1.737869959597756697 ) ) ;
#10447 = PLANE ( 'NONE',  #9792 ) ;
#10448 = DIRECTION ( 'NONE',  ( 1.000000000000000000, 0.000000000000000000, -0.000000000000000000 ) ) ;
#10449 = ADVANCED_FACE ( 'NONE', ( #6328 ), #6271, .F. ) ;
#10450 = ORIENTED_EDGE ( 'NONE', *, *, #5797, .T. ) ;
#10451 = ADVANCED_FACE ( 'NONE', ( #18547 ), #3239, .F. ) ;
#10452 = CARTESIAN_POINT ( 'NONE',  ( 1.039999999999999147, 12.52377138324259676, -25.12109765559640095 ) ) ;
#10453 = CIRCLE ( 'NONE', #12050, 1.000000000000004441 ) ;
#10454 = CARTESIAN_POINT ( 'NONE',  ( 0.000000000000000000, 24.04302995059966719, 1.991882183130389228 ) ) ;
#10455 = ADVANCED_FACE ( 'NONE', ( #5131 ), #14250, .F. ) ;
#10456 = ORIENTED_EDGE ( 'NONE', *, *, #14578, .T. ) ;
#10457 = DIRECTION ( 'NONE',  ( 1.000000000000000000, 0.000000000000000000, 0.000000000000000000 ) ) ;
#10458 = DIRECTION ( 'NONE',  ( 0.000000000000000000, -1.224646799147353207E-16, 1.000000000000000000 ) ) ;
#10459 = VERTEX_POINT ( 'NONE', #3346 ) ;
#10460 = DIRECTION ( 'NONE',  ( 0.000000000000000000, 1.000000000000000000, -1.224646799147353207E-16 ) ) ;
#10461 = DIRECTION ( 'NONE',  ( 0.000000000000000000, 0.000000000000000000, 1.000000000000000000 ) ) ;
#10462 = DIRECTION ( 'NONE',  ( 0.000000000000000000, 0.000000000000000000, 1.000000000000000000 ) ) ;
#10463 = ORIENTED_EDGE ( 'NONE', *, *, #13868, .F. ) ;
#10464 = CARTESIAN_POINT ( 'NONE',  ( 7.968749997951616315, -4.942249507334558700, 0.2590123213420630899 ) ) ;
#10465 = CIRCLE ( 'NONE', #1833, 0.9999999999999974465 ) ;
#10466 = ORIENTED_EDGE ( 'NONE', *, *, #2457, .T. ) ;
#10467 = DIRECTION ( 'NONE',  ( 0.9029554308451981370, -0.4297342084441994059, 7.518614321510043780E-17 ) ) ;
#10468 = CARTESIAN_POINT ( 'NONE',  ( 2.068159791354145849, -5.387740456496247887, -6.500000000000005329 ) ) ;
#10469 = AXIS2_PLACEMENT_3D ( 'NONE', #3949, #14851, #3849 ) ;
#10470 = VERTEX_POINT ( 'NONE', #1843 ) ;
#10471 = ORIENTED_EDGE ( 'NONE', *, *, #13974, .T. ) ;
#10472 = DIRECTION ( 'NONE',  ( 1.000000000000000000, 0.000000000000000000, 0.000000000000000000 ) ) ;
#10473 = APPLICATION_CONTEXT ( 'automotive_design' ) ;
#10474 = DIRECTION ( 'NONE',  ( 1.000000000000000000, 0.000000000000000000, 0.000000000000000000 ) ) ;
#10475 = ORIENTED_EDGE ( 'NONE', *, *, #216, .T. ) ;
#10476 = EDGE_CURVE ( 'NONE', #600, #16700, #6885, .T. ) ;
#10477 = CARTESIAN_POINT ( 'NONE',  ( -17.28688694438836393, -7.664027248171298545, -35.00000000000000000 ) ) ;
#10478 = ORIENTED_EDGE ( 'NONE', *, *, #8664, .F. ) ;
#10479 = CARTESIAN_POINT ( 'NONE',  ( -25.31088913245540084, -1.027644533213482535E-13, 37.99999999999999289 ) ) ;
#10480 = CARTESIAN_POINT ( 'NONE',  ( 9.671566133830877376, 15.77352024078954784, 35.00000000000000000 ) ) ;
#10481 = VECTOR ( 'NONE', #627, 1000.000000000000000 ) ;
#10482 = EDGE_LOOP ( 'NONE', ( #5620, #19118 ) ) ;
#10483 = ADVANCED_FACE ( 'NONE', ( #7014 ), #17452, .F. ) ;
#10484 = AXIS2_PLACEMENT_3D ( 'NONE', #4908, #18904, #1901 ) ;
#10485 = LINE ( 'NONE', #15082, #6152 ) ;
#10486 = CARTESIAN_POINT ( 'NONE',  ( 2.789999999999999147, 2.336989772644613161, -24.63872515616080250 ) ) ;
#10487 = CARTESIAN_POINT ( 'NONE',  ( 5.700000000000001066, -3.980288726281172656E-14, -7.312499995903225525 ) ) ;
#10488 = ORIENTED_EDGE ( 'NONE', *, *, #18616, .T. ) ;
#10489 = ADVANCED_FACE ( 'NONE', ( #4130 ), #2139, .F. ) ;
#10490 = CARTESIAN_POINT ( 'NONE',  ( -7.626241948324210540, -16.73597674598852336, 32.00000000000000000 ) ) ;
#10491 = SURFACE_SIDE_STYLE ('',( #4380 ) ) ;
#10492 = ORIENTED_EDGE ( 'NONE', *, *, #12312, .F. ) ;
#10493 = CARTESIAN_POINT ( 'NONE',  ( 16.28688694438835327, -7.664027248171309203, 32.00000000000000000 ) ) ;
#10494 = CIRCLE ( 'NONE', #2808, 24.12539914357697413 ) ;
#10495 = CARTESIAN_POINT ( 'NONE',  ( 2.789999999999999147, 20.70663861606293210, -12.51925356660738053 ) ) ;
#10496 = CARTESIAN_POINT ( 'NONE',  ( -7.626241948324210540, -16.73597674598852336, -32.00000000000000000 ) ) ;
#10497 = AXIS2_PLACEMENT_3D ( 'NONE', #17581, #17777, #10086 ) ;
#10498 = DIRECTION ( 'NONE',  ( 1.000000000000000000, 0.000000000000000000, 0.000000000000000000 ) ) ;
#10499 = DIRECTION ( 'NONE',  ( 0.000000000000000000, 0.000000000000000000, 1.000000000000000000 ) ) ;
#10500 = ORIENTED_EDGE ( 'NONE', *, *, #13305, .F. ) ;
#10501 = LINE ( 'NONE', #7475, #8673 ) ;
#10502 =( BOUNDED_CURVE ( )  B_SPLINE_CURVE ( 2, ( #13928, #221, #7509, #19727, #10633, #16738, #3017, #15237, #6113, #7910, #8009, #12529, #6500, #14225, #6598, #8315, #14325 ),
 .UNSPECIFIED., .F., .F. ) 
 B_SPLINE_CURVE_WITH_KNOTS ( ( 3, 2, 2, 2, 2, 2, 2, 2, 3 ),
 ( 0.000000000000000000, 0.05000000000000000971, 0.1000000000000000194, 0.1499999999999999944, 0.2000000000000000389, 0.2500000000000000000, 0.2999999999999999889, 0.3499999999999999223, 0.4000000000000000777 ),
 .UNSPECIFIED. ) 
 CURVE ( )  GEOMETRIC_REPRESENTATION_ITEM ( )  RATIONAL_B_SPLINE_CURVE ( ( 1.000000000000000000, 0.9876883405951377704, 1.000000000000000000, 0.9876883405951377704, 1.000000000000000000, 0.9876883405951377704, 1.000000000000000000, 0.9876883405951377704, 1.000000000000000000, 0.9876883405951377704, 1.000000000000000000, 0.9876883405951377704, 1.000000000000000000, 0.9876883405951377704, 1.000000000000000000, 0.9876883405951377704, 1.000000000000000000 ) ) 
 REPRESENTATION_ITEM ( '' )  );
#10503 = CARTESIAN_POINT ( 'NONE',  ( -3.632567103900569361, -3.270778111535287191, -7.468749997951615427 ) ) ;
#10504 = VERTEX_POINT ( 'NONE', #2424 ) ;
#10505 = ADVANCED_FACE ( 'NONE', ( #16154, #12847 ), #11733, .T. ) ;
#10506 = CARTESIAN_POINT ( 'NONE',  ( 2.000000000000001776, 0.000000000000000000, 0.000000000000000000 ) ) ;
#10507 = CIRCLE ( 'NONE', #9880, 1.000000000000000888 ) ;
#10508 = LINE ( 'NONE', #9002, #6135 ) ;
#10509 = CARTESIAN_POINT ( 'NONE',  ( -2.602085213965210642E-14, -9.165435523385315975, -0.7089489049740167470 ) ) ;
#10510 = ORIENTED_EDGE ( 'NONE', *, *, #14366, .F. ) ;
#10511 = CARTESIAN_POINT ( 'NONE',  ( -15.00000000000000355, 8.000000000000000000, 0.000000000000000000 ) ) ;
#10512 = FACE_OUTER_BOUND ( 'NONE', #649, .T. ) ;
#10513 = CARTESIAN_POINT ( 'NONE',  ( 6.626241948324199882, -16.73597674598852691, 32.00000000000000000 ) ) ;
#10514 = VERTEX_POINT ( 'NONE', #4034 ) ;
#10515 = DIRECTION ( 'NONE',  ( 1.000000000000000000, 0.000000000000000000, 0.000000000000000000 ) ) ;
#10516 = CARTESIAN_POINT ( 'NONE',  ( 7.968749997951616315, -2.246813503491864150, 4.409619785863891472 ) ) ;
#10517 = CARTESIAN_POINT ( 'NONE',  ( -10.00000000000000000, 0.000000000000000000, 0.000000000000000000 ) ) ;
#10518 = EDGE_CURVE ( 'NONE', #7592, #1723, #208, .T. ) ;
#10519 = EDGE_CURVE ( 'NONE', #488, #4769, #1557, .T. ) ;
#10520 = CARTESIAN_POINT ( 'NONE',  ( 2.789999999999999147, -9.324097380959603498, 22.25075486061734864 ) ) ;
#10521 = AXIS2_PLACEMENT_3D ( 'NONE', #10741, #14306, #17306 ) ;
#10522 = CARTESIAN_POINT ( 'NONE',  ( -17.68117051311639898, -3.372863662543042818, -32.00000000000000000 ) ) ;
#10523 = ORIENTED_EDGE ( 'NONE', *, *, #423, .F. ) ;
#10524 = CARTESIAN_POINT ( 'NONE',  ( 0.2590123213420631454, -4.942249507334558700, -7.968749997951616315 ) ) ;
#10525 = CARTESIAN_POINT ( 'NONE',  ( 2.601776096565022289, 22.54313264455032240, -12.84621645676820201 ) ) ;
#10526 = ORIENTED_EDGE ( 'NONE', *, *, #13974, .F. ) ;
#10527 = EDGE_CURVE ( 'NONE', #15763, #2089, #4761, .T. ) ;
#10528 = CARTESIAN_POINT ( 'NONE',  ( -2.246813503491833508, 4.409619785863906571, -9.968749997951617203 ) ) ;
#10529 = CARTESIAN_POINT ( 'NONE',  ( -1.799999999999999600, 0.000000000000000000, -8.000000000000000000 ) ) ;
#10530 = ORIENTED_EDGE ( 'NONE', *, *, #13662, .F. ) ;
#10531 = LINE ( 'NONE', #3292, #1092 ) ;
#10532 = LINE ( 'NONE', #18043, #4346 ) ;
#10533 = LINE ( 'NONE', #18239, #17073 ) ;
#10534 = ORIENTED_EDGE ( 'NONE', *, *, #10676, .T. ) ;
#10535 = CARTESIAN_POINT ( 'NONE',  ( -2.000000000000000000, -8.000000000000003553, 37.99999999999999289 ) ) ;
#10536 = ORIENTED_EDGE ( 'NONE', *, *, #12150, .T. ) ;
#10537 = CARTESIAN_POINT ( 'NONE',  ( -1.310841663519413114, 0.000000000000000000, 0.000000000000000000 ) ) ;
#10538 = ORIENTED_EDGE ( 'NONE', *, *, #3875, .F. ) ;
#10539 = MECHANICAL_DESIGN_GEOMETRIC_PRESENTATION_REPRESENTATION (  '', ( #13089 ), #15650 ) ;
#10540 = CARTESIAN_POINT ( 'NONE',  ( 89.62500000000000000, 0.000000000000000000, 0.000000000000000000 ) ) ;
#10541 = CARTESIAN_POINT ( 'NONE',  ( 2.358581579527286198, -23.43037373958380343, 12.94152279942367656 ) ) ;
#10542 = DIRECTION ( 'NONE',  ( 0.000000000000000000, 0.000000000000000000, -1.000000000000000000 ) ) ;
#10543 = CARTESIAN_POINT ( 'NONE',  ( 7.468749997951615427, -4.781284448697200595, 1.016293382781377819 ) ) ;
#10544 = CARTESIAN_POINT ( 'NONE',  ( 0.07186813532171169860, -2.577209017047189299, 25.22589920183361301 ) ) ;
#10545 = VERTEX_POINT ( 'NONE', #2334 ) ;
#10546 = CYLINDRICAL_SURFACE ( 'NONE', #15705, 2.524999999999995914 ) ;
#10547 = CARTESIAN_POINT ( 'NONE',  ( -22.00000000000000355, 0.000000000000000000, -35.00000000000000000 ) ) ;
#10548 = EDGE_CURVE ( 'NONE', #14863, #2115, #8449, .T. ) ;
#10549 = EDGE_CURVE ( 'NONE', #9689, #7585, #4984, .T. ) ;
#10550 = CIRCLE ( 'NONE', #9269, 2.524999999999996358 ) ;
#10551 = VERTEX_POINT ( 'NONE', #18137 ) ;
#10552 = B_SPLINE_CURVE_WITH_KNOTS ( 'NONE', 3,
 ( #15004, #10600, #16706, #13299 ),
 .UNSPECIFIED., .F., .F.,
 ( 4, 4 ),
 ( 2.034713381942769504E-07, 0.0006887909409525124101 ),
 .UNSPECIFIED. ) ;
#10553 = CIRCLE ( 'NONE', #17264, 4.000000000000000000 ) ;
#10554 = DIRECTION ( 'NONE',  ( -1.000000000000000000, -0.000000000000000000, -0.000000000000000000 ) ) ;
#10555 = CARTESIAN_POINT ( 'NONE',  ( 6.000000000000005329, 0.000000000000000000, 0.000000000000000000 ) ) ;
#10556 = VERTEX_POINT ( 'NONE', #5914 ) ;
#10557 = LINE ( 'NONE', #6036, #12492 ) ;
#10558 = CARTESIAN_POINT ( 'NONE',  ( 4.500000000000000000, 5.510910596163088569E-16, -33.00000000000000000 ) ) ;
#10559 = FACE_OUTER_BOUND ( 'NONE', #15341, .T. ) ;
#10560 = ORIENTED_EDGE ( 'NONE', *, *, #11443, .T. ) ;
#10561 = EDGE_CURVE ( 'NONE', #14057, #17046, #5714, .T. ) ;
#10562 = CARTESIAN_POINT ( 'NONE',  ( 8.968749997951613651, -4.780397808154247308, -1.280903732194487166 ) ) ;
#10563 = EDGE_LOOP ( 'NONE', ( #1566, #13296, #6893, #8627 ) ) ;
#10564 = DIRECTION ( 'NONE',  ( 0.000000000000000000, 0.000000000000000000, -1.000000000000000000 ) ) ;
#10565 = DIRECTION ( 'NONE',  ( 1.000000000000000000, 0.000000000000000000, 0.000000000000000000 ) ) ;
#10566 = DIRECTION ( 'NONE',  ( 0.000000000000000000, 0.000000000000000000, 1.000000000000000000 ) ) ;
#10567 = ORIENTED_EDGE ( 'NONE', *, *, #6736, .F. ) ;
#10568 = ORIENTED_EDGE ( 'NONE', *, *, #14385, .F. ) ;
#10569 = DIRECTION ( 'NONE',  ( -0.000000000000000000, -0.000000000000000000, 1.000000000000000000 ) ) ;
#10570 = VECTOR ( 'NONE', #702, 1000.000000000000000 ) ;
#10571 = CARTESIAN_POINT ( 'NONE',  ( 4.620319390059829168, 1.773574444220725743, -12.34374999795161543 ) ) ;
#10572 = ADVANCED_FACE ( 'NONE', ( #10243 ), #18556, .F. ) ;
#10573 = AXIS2_PLACEMENT_3D ( 'NONE', #13906, #16914, #1796 ) ;
#10574 = ORIENTED_EDGE ( 'NONE', *, *, #6032, .F. ) ;
#10575 = CARTESIAN_POINT ( 'NONE',  ( 0.000000000000000000, 0.000000000000000000, -29.00000000000000000 ) ) ;
#10576 = ORIENTED_EDGE ( 'NONE', *, *, #1481, .T. ) ;
#10577 = DIRECTION ( 'NONE',  ( 0.000000000000000000, 0.000000000000000000, 1.000000000000000000 ) ) ;
#10578 = ORIENTED_EDGE ( 'NONE', *, *, #378, .F. ) ;
#10579 = VECTOR ( 'NONE', #8603, 1000.000000000000000 ) ;
#10580 = CARTESIAN_POINT ( 'NONE',  ( 3.476417968967386418, 17.43449690031536292, -32.00000000000000000 ) ) ;
#10581 = ADVANCED_FACE ( 'NONE', ( #1131 ), #4228, .T. ) ;
#10582 = FACE_OUTER_BOUND ( 'NONE', #19354, .T. ) ;
#10583 = CARTESIAN_POINT ( 'NONE',  ( 14.19790265903627180, 9.644882309621939598, -32.00000000000000000 ) ) ;
#10584 = ORIENTED_EDGE ( 'NONE', *, *, #18760, .F. ) ;
#10585 = DIRECTION ( 'NONE',  ( -0.9238795325112865164, 0.3826834323650905034, 0.000000000000000000 ) ) ;
#10586 = DIRECTION ( 'NONE',  ( 1.000000000000000000, 0.000000000000000000, 0.000000000000000000 ) ) ;
#10587 = ORIENTED_EDGE ( 'NONE', *, *, #18006, .F. ) ;
#10588 = DIRECTION ( 'NONE',  ( 0.000000000000000000, 0.000000000000000000, 1.000000000000000000 ) ) ;
#10589 = CARTESIAN_POINT ( 'NONE',  ( -2.000000000000001776, 0.000000000000000000, 0.000000000000000000 ) ) ;
#10590 = PRODUCT_DEFINITION_CONTEXT ( 'detailed design', #7370, 'design' ) ;
#10591 = CARTESIAN_POINT ( 'NONE',  ( 2.789999999999999147, -7.909232158574647009, -24.34211360614308006 ) ) ;
#10592 = DIRECTION ( 'NONE',  ( 0.000000000000000000, 0.000000000000000000, -1.000000000000000000 ) ) ;
#10593 = LINE ( 'NONE', #9194, #1862 ) ;
#10594 = AXIS2_PLACEMENT_3D ( 'NONE', #17679, #3973, #19740 ) ;
#10595 = ORIENTED_EDGE ( 'NONE', *, *, #9057, .F. ) ;
#10596 = DIRECTION ( 'NONE',  ( -1.000000000000000000, -0.000000000000000000, 0.000000000000000000 ) ) ;
#10597 = CARTESIAN_POINT ( 'NONE',  ( 2.765633920072239516, -24.63872515616084513, 2.336989772644183283 ) ) ;
#10598 = ORIENTED_EDGE ( 'NONE', *, *, #19004, .F. ) ;
#10599 = CARTESIAN_POINT ( 'NONE',  ( 8.312499995903225525, 3.814044456245473835, 4.235925505221166176 ) ) ;
#10600 = CARTESIAN_POINT ( 'NONE',  ( 0.006974663525959075641, 12.53640742967783694, -21.08118142846890208 ) ) ;
#10601 = B_SPLINE_CURVE_WITH_KNOTS ( 'NONE', 3,
 ( #8832, #11829, #7507, #2814 ),
 .UNSPECIFIED., .F., .F.,
 ( 4, 4 ),
 ( 2.135345996175579449E-07, 0.0006888010880210803950 ),
 .UNSPECIFIED. ) ;
#10602 = DIRECTION ( 'NONE',  ( 1.000000000000000000, 0.000000000000000000, 0.000000000000000000 ) ) ;
#10603 = CARTESIAN_POINT ( 'NONE',  ( -2.624839991567115227, -7.649983447674356007, -0.06756670027994669814 ) ) ;
#10604 = ORIENTED_EDGE ( 'NONE', *, *, #7750, .F. ) ;
#10605 = CIRCLE ( 'NONE', #5478, 24.12539914357697413 ) ;
#10606 = VECTOR ( 'NONE', #2780, 1000.000000000000000 ) ;
#10607 = CARTESIAN_POINT ( 'NONE',  ( -2.300000000000000711, 0.000000000000000000, 0.000000000000000000 ) ) ;
#10608 = CARTESIAN_POINT ( 'NONE',  ( -17.11901729331276911, 5.562305898749051458, -32.00000000000000000 ) ) ;
#10609 = AXIS2_PLACEMENT_3D ( 'NONE', #6810, #5415, #12832 ) ;
#10610 = CARTESIAN_POINT ( 'NONE',  ( 11.50000000000000355, -5.699999999999994849, -0.9027913098498961952 ) ) ;
#10611 = ORIENTED_EDGE ( 'NONE', *, *, #14160, .T. ) ;
#10612 = DIRECTION ( 'NONE',  ( -1.000000000000000000, -0.000000000000000000, -0.000000000000000000 ) ) ;
#10613 = DIRECTION ( 'NONE',  ( 0.000000000000000000, 0.000000000000000000, 1.000000000000000000 ) ) ;
#10614 = CARTESIAN_POINT ( 'NONE',  ( 2.789895169984651702, -20.67846228565646172, -12.51925356660783528 ) ) ;
#10615 = EDGE_CURVE ( 'NONE', #16727, #3453, #10532, .T. ) ;
#10616 = CIRCLE ( 'NONE', #13170, 2.524999999999995914 ) ;
#10617 = CARTESIAN_POINT ( 'NONE',  ( 10.84374999795161543, 4.648860486681953397, -1.510506337161861667 ) ) ;
#10618 = FACE_OUTER_BOUND ( 'NONE', #16280, .T. ) ;
#10619 = DIRECTION ( 'NONE',  ( 1.000000000000000000, 0.000000000000000000, 0.000000000000000000 ) ) ;
#10620 = ORIENTED_EDGE ( 'NONE', *, *, #15421, .F. ) ;
#10621 = CARTESIAN_POINT ( 'NONE',  ( 2.765633920072238627, 5.391175441198956086, -24.15498966839956907 ) ) ;
#10622 = CARTESIAN_POINT ( 'NONE',  ( -36.00000000000000000, -4.200000000000000178, 0.000000000000000000 ) ) ;
#10623 = CIRCLE ( 'NONE', #6437, 0.9999999999999974465 ) ;
#10624 = VERTEX_POINT ( 'NONE', #7205 ) ;
#10625 = VECTOR ( 'NONE', #16580, 1000.000000000000000 ) ;
#10626 = AXIS2_PLACEMENT_3D ( 'NONE', #12187, #1685, #7869 ) ;
#10627 = CIRCLE ( 'NONE', #1997, 6.799999999999998934 ) ;
#10628 = EDGE_CURVE ( 'NONE', #6807, #13831, #12021, .T. ) ;
#10629 = CARTESIAN_POINT ( 'NONE',  ( 3.954556930911842016, -2.873153789725853002, -8.843749997951615427 ) ) ;
#10630 = VERTEX_POINT ( 'NONE', #16440 ) ;
#10631 = CARTESIAN_POINT ( 'NONE',  ( 3.270778111535338262, 3.632567103900523620, -10.46874999795161720 ) ) ;
#10632 = CARTESIAN_POINT ( 'NONE',  ( 8.343749997951611874, 4.942249507334556924, -0.2590123213420975623 ) ) ;
#10633 = CARTESIAN_POINT ( 'NONE',  ( -3.954556930911862000, 2.873153789725825469, -8.468749997951615427 ) ) ;
#10634 = ORIENTED_EDGE ( 'NONE', *, *, #6981, .T. ) ;
#10635 = DIRECTION ( 'NONE',  ( 0.9773501006361904331, 0.000000000000000000, -0.2116288751244229938 ) ) ;
#10636 = VERTEX_POINT ( 'NONE', #1225 ) ;
#10637 = CARTESIAN_POINT ( 'NONE',  ( -5.645569974854468320, -5.905964178674223852, -0.1296323192022640625 ) ) ;
#10638 = ORIENTED_EDGE ( 'NONE', *, *, #777, .F. ) ;
#10639 = CARTESIAN_POINT ( 'NONE',  ( 2.783025325906567371, 2.249040938978837278, -24.42374957165203142 ) ) ;
#10640 = ADVANCED_FACE ( 'NONE', ( #2716 ), #8833, .F. ) ;
#10641 = CIRCLE ( 'NONE', #17666, 7.800000000000000711 ) ;
#10642 = CARTESIAN_POINT ( 'NONE',  ( 5.294050593750000644, -3.696815770993907903E-14, -6.234374998975811266 ) ) ;
#10643 = CARTESIAN_POINT ( 'NONE',  ( 9.580134541264516912, -14.56230589874905412, 35.00000000000000000 ) ) ;
#10644 = CYLINDRICAL_SURFACE ( 'NONE', #18709, 1.000000000000002665 ) ;
#10645 = CIRCLE ( 'NONE', #5205, 3.323499999999993015 ) ;
#10646 = CARTESIAN_POINT ( 'NONE',  ( 8.468749997951615427, 4.861323657744407001, 0.5109457054261784537 ) ) ;
#10647 = VERTEX_POINT ( 'NONE', #16539 ) ;
#10648 = AXIS2_PLACEMENT_3D ( 'NONE', #6170, #19777, #5967 ) ;
#10649 = DIRECTION ( 'NONE',  ( 0.000000000000000000, 0.000000000000000000, -1.000000000000000000 ) ) ;
#10650 =( REPRESENTATION_RELATIONSHIP ('NONE','NONE', #18211, #6040 ) REPRESENTATION_RELATIONSHIP_WITH_TRANSFORMATION ( #16160 )SHAPE_REPRESENTATION_RELATIONSHIP( ) );
#10651 = CARTESIAN_POINT ( 'NONE',  ( 1.039999999999995817, 4.633866840648921404, 27.68468304288260029 ) ) ;
#10652 = VECTOR ( 'NONE', #6697, 1000.000000000000000 ) ;
#10653 = ORIENTED_EDGE ( 'NONE', *, *, #16064, .T. ) ;
#10654 = DIRECTION ( 'NONE',  ( -0.000000000000000000, -0.000000000000000000, 1.000000000000000000 ) ) ;
#10655 = EDGE_CURVE ( 'NONE', #1107, #6633, #5931, .T. ) ;
#10656 = DIRECTION ( 'NONE',  ( 0.000000000000000000, 0.000000000000000000, -1.000000000000000000 ) ) ;
#10657 = VERTEX_POINT ( 'NONE', #8008 ) ;
#10658 = DIRECTION ( 'NONE',  ( 0.000000000000000000, 0.000000000000000000, 1.000000000000000000 ) ) ;
#10659 = CARTESIAN_POINT ( 'NONE',  ( 5.763142191869155440, -0.3020334839682879413, -9.500000000000003553 ) ) ;
#10660 = CIRCLE ( 'NONE', #4583, 28.06981291497571362 ) ;
#10661 = ORIENTED_EDGE ( 'NONE', *, *, #1956, .F. ) ;
#10662 = FACE_OUTER_BOUND ( 'NONE', #19321, .T. ) ;
#10663 = EDGE_CURVE ( 'NONE', #5291, #15288, #13422, .T. ) ;
#10664 = CARTESIAN_POINT ( 'NONE',  ( 0.000000000000000000, 23.48180575137739368, -5.535312321042471062 ) ) ;
#10665 = LINE ( 'NONE', #18364, #19156 ) ;
#10666 = ORIENTED_EDGE ( 'NONE', *, *, #3708, .T. ) ;
#10667 = VERTEX_POINT ( 'NONE', #10729 ) ;
#10668 = EDGE_CURVE ( 'NONE', #1940, #4236, #71, .T. ) ;
#10669 = CARTESIAN_POINT ( 'NONE',  ( 0.02436607992776151574, 24.15498966839970052, -5.391175441198366336 ) ) ;
#10670 = MECHANICAL_DESIGN_GEOMETRIC_PRESENTATION_REPRESENTATION (  '', ( #17051 ), #16419 ) ;
#10671 = CARTESIAN_POINT ( 'NONE',  ( -1.185096637661215535, 5.575441324182696334, -8.312499995903225525 ) ) ;
#10672 = ORIENTED_EDGE ( 'NONE', *, *, #17243, .F. ) ;
#10673 = DIRECTION ( 'NONE',  ( -1.000000000000000000, 1.224646799147353207E-16, 0.000000000000000000 ) ) ;
#10674 = ORIENTED_EDGE ( 'NONE', *, *, #9651, .T. ) ;
#10675 = CARTESIAN_POINT ( 'NONE',  ( -2.000000000000001776, -3.218695387886217674, 2.999999999999999112 ) ) ;
#10676 = EDGE_CURVE ( 'NONE', #16730, #2850, #121, .T. ) ;
#10677 = ORIENTED_EDGE ( 'NONE', *, *, #14586, .F. ) ;
#10678 = AXIS2_PLACEMENT_3D ( 'NONE', #3835, #18944, #2520 ) ;
#10679 = EDGE_CURVE ( 'NONE', #9247, #15763, #3419, .T. ) ;
#10680 = DIRECTION ( 'NONE',  ( -0.000000000000000000, -0.000000000000000000, 1.000000000000000000 ) ) ;
#10681 = CARTESIAN_POINT ( 'NONE',  ( 11.84374999795161365, 4.888101187500000222, -2.993098736590125853E-16 ) ) ;
#10682 = DIRECTION ( 'NONE',  ( 0.000000000000000000, 0.000000000000000000, 1.000000000000000000 ) ) ;
#10683 = EDGE_LOOP ( 'NONE', ( #14526, #19512, #2615, #12202, #19237, #12752, #1227, #14328 ) ) ;
#10684 = PLANE ( 'NONE',  #3418 ) ;
#10685 = CARTESIAN_POINT ( 'NONE',  ( 0.000000000000000000, -22.25075486061732732, -9.324097380959701198 ) ) ;
#10686 = AXIS2_PLACEMENT_3D ( 'NONE', #9863, #6623, #18472 ) ;
#10687 = ORIENTED_EDGE ( 'NONE', *, *, #3282, .T. ) ;
#10688 = CARTESIAN_POINT ( 'NONE',  ( -2.000000000000001776, 0.000000000000000000, 0.000000000000000000 ) ) ;
#10689 = CARTESIAN_POINT ( 'NONE',  ( 2.789999999999999147, -19.64056340710864745, -14.55412442567638287 ) ) ;
#10690 = EDGE_CURVE ( 'NONE', #6978, #18537, #1164, .T. ) ;
#10691 = DIRECTION ( 'NONE',  ( -0.000000000000000000, -0.000000000000000000, 1.000000000000000000 ) ) ;
#10692 = CARTESIAN_POINT ( 'NONE',  ( -15.00000000000000355, 4.874999999999997335, -3.903123748998999609 ) ) ;
#10693 = CIRCLE ( 'NONE', #10066, 1.000000000000004441 ) ;
#10694 = CARTESIAN_POINT ( 'NONE',  ( -0.7741991708318890497, 4.888101187500000222, -11.34374999795161543 ) ) ;
#10695 = ORIENTED_EDGE ( 'NONE', *, *, #16003, .T. ) ;
#10696 = DIRECTION ( 'NONE',  ( -1.000000000000000000, -0.000000000000000000, 0.000000000000000000 ) ) ;
#10697 = EDGE_CURVE ( 'NONE', #619, #10459, #13896, .T. ) ;
#10698 = CARTESIAN_POINT ( 'NONE',  ( 13.00000000000000533, -0.5958122406256377568, 5.668774803599156975 ) ) ;
#10699 = ORIENTED_EDGE ( 'NONE', *, *, #16372, .T. ) ;
#10700 = CARTESIAN_POINT ( 'NONE',  ( 9.500000000000003553, 0.3020334839683282979, -5.763142191869152775 ) ) ;
#10701 = CIRCLE ( 'NONE', #6199, 4.000000000000000000 ) ;
#10702 = LINE ( 'NONE', #19399, #18559 ) ;
#10703 = DIRECTION ( 'NONE',  ( 0.000000000000000000, 0.000000000000000000, 1.000000000000000000 ) ) ;
#10704 = DIRECTION ( 'NONE',  ( -1.000000000000000000, -0.000000000000000000, -0.000000000000000000 ) ) ;
#10705 = ORIENTED_EDGE ( 'NONE', *, *, #9812, .T. ) ;
#10706 = AXIS2_PLACEMENT_3D ( 'NONE', #5639, #8747, #16353 ) ;
#10707 = CARTESIAN_POINT ( 'NONE',  ( 6.000000000000005329, 0.000000000000000000, -5.700000000000001066 ) ) ;
#10708 =( NAMED_UNIT ( * ) PLANE_ANGLE_UNIT ( ) SI_UNIT ( $, .RADIAN. ) );
#10709 = LINE ( 'NONE', #7689, #5568 ) ;
#10710 = CARTESIAN_POINT ( 'NONE',  ( 1.749999999999998002, 12.96210679857822257, -24.89775460606818669 ) ) ;
#10711 = ORIENTED_EDGE ( 'NONE', *, *, #19608, .T. ) ;
#10712 = DIRECTION ( 'NONE',  ( 0.000000000000000000, 0.000000000000000000, 1.000000000000000000 ) ) ;
#10713 = CARTESIAN_POINT ( 'NONE',  ( 2.765633920072234631, -21.30679549418640306, 12.59161484032904887 ) ) ;
#10714 = CARTESIAN_POINT ( 'NONE',  ( 7.500000000000005329, 5.763142191869157216, -0.3020334839682475847 ) ) ;
#10715 = CYLINDRICAL_SURFACE ( 'NONE', #1192, 1.000000000000004441 ) ;
#10716 = ORIENTED_EDGE ( 'NONE', *, *, #6565, .F. ) ;
#10717 = LINE ( 'NONE', #9519, #12524 ) ;
#10718 = CARTESIAN_POINT ( 'NONE',  ( -12.86923836996420611, -11.47363181547641275, -35.00000000000000000 ) ) ;
#10719 = ORIENTED_EDGE ( 'NONE', *, *, #18156, .F. ) ;
#10720 = ADVANCED_FACE ( 'NONE', ( #3215 ), #13829, .F. ) ;
#10721 = CARTESIAN_POINT ( 'NONE',  ( 10.84374999795161543, -4.648860486681964055, 1.510506337161829027 ) ) ;
#10722 = CARTESIAN_POINT ( 'NONE',  ( 0.02436607992775978102, 24.63872515616082737, 2.336989772644355146 ) ) ;
#10723 = AXIS2_PLACEMENT_3D ( 'NONE', #17463, #19056, #7025 ) ;
#10724 = ORIENTED_EDGE ( 'NONE', *, *, #15596, .F. ) ;
#10725 = EDGE_CURVE ( 'NONE', #5656, #19204, #7203, .T. ) ;
#10726 = LINE ( 'NONE', #1423, #3569 ) ;
#10727 = CARTESIAN_POINT ( 'NONE',  ( 1.039999999999997593, -12.52377138324241557, 25.12109765559648977 ) ) ;
#10728 = ORIENTED_EDGE ( 'NONE', *, *, #6593, .F. ) ;
#10729 = CARTESIAN_POINT ( 'NONE',  ( -25.31088913245573835, 82.80384757729319745, 41.99999999999999289 ) ) ;
#10730 = DIRECTION ( 'NONE',  ( 0.000000000000000000, 0.000000000000000000, 1.000000000000000000 ) ) ;
#10731 = ORIENTED_EDGE ( 'NONE', *, *, #16768, .T. ) ;
#10732 = FACE_OUTER_BOUND ( 'NONE', #18182, .T. ) ;
#10733 = ORIENTED_EDGE ( 'NONE', *, *, #731, .T. ) ;
#10734 = CARTESIAN_POINT ( 'NONE',  ( -7.755480735455585059E-14, 24.22524813288762502, -2.133839912090887303 ) ) ;
#10735 = CIRCLE ( 'NONE', #17121, 24.12539914357697413 ) ;
#10736 = ORIENTED_EDGE ( 'NONE', *, *, #5772, .T. ) ;
#10737 = ADVANCED_FACE ( 'NONE', ( #6498 ), #6596, .F. ) ;
#10738 = DIRECTION ( 'NONE',  ( 1.000000000000000000, 0.000000000000000000, 0.000000000000000000 ) ) ;
#10739 = AXIS2_PLACEMENT_3D ( 'NONE', #12645, #6815, #11343 ) ;
#10740 = CARTESIAN_POINT ( 'NONE',  ( 2.765633920072234631, -21.30679549418640306, 12.59161484032904887 ) ) ;
#10741 = CARTESIAN_POINT ( 'NONE',  ( -2.255998204157477538, -17.85806462366060288, -32.00000000000000000 ) ) ;
#10742 = CARTESIAN_POINT ( 'NONE',  ( 2.789999999999999147, -15.04425356660744839, -20.70663861606288236 ) ) ;
#10743 = LINE ( 'NONE', #3131, #15269 ) ;
#10744 = VERTEX_POINT ( 'NONE', #1817 ) ;
#10745 = FACE_OUTER_BOUND ( 'NONE', #7185, .T. ) ;
#10746 = DIRECTION ( 'NONE',  ( 0.000000000000000000, 0.000000000000000000, 1.000000000000000000 ) ) ;
#10747 = AXIS2_PLACEMENT_3D ( 'NONE', #8608, #10029, #912 ) ;
#10748 = CARTESIAN_POINT ( 'NONE',  ( 6.234374998975811266, -4.584782303107616031, 2.647025296874957689 ) ) ;
#10749 = EDGE_CURVE ( 'NONE', #881, #18268, #14264, .T. ) ;
#10750 = VECTOR ( 'NONE', #7006, 1000.000000000000000 ) ;
#10751 = DIRECTION ( 'NONE',  ( 0.000000000000000000, 0.000000000000000000, -1.000000000000000000 ) ) ;
#10752 = CARTESIAN_POINT ( 'NONE',  ( 0.000000000000000000, 7.347880794884119736E-16, -6.000000000000000000 ) ) ;
#10753 = ORIENTED_EDGE ( 'NONE', *, *, #13238, .F. ) ;
#10754 = CARTESIAN_POINT ( 'NONE',  ( 2.718184743034448569, 24.78695292654929005, -5.344212458769106888 ) ) ;
#10755 = DIRECTION ( 'NONE',  ( 0.000000000000000000, 0.000000000000000000, 1.000000000000000000 ) ) ;
#10756 = ORIENTED_EDGE ( 'NONE', *, *, #5982, .F. ) ;
#10757 = CARTESIAN_POINT ( 'NONE',  ( -5.000000000000000000, 0.000000000000000000, 37.99999999999999289 ) ) ;
#10758 = ORIENTED_EDGE ( 'NONE', *, *, #1048, .T. ) ;
#10759 = SHAPE_DEFINITION_REPRESENTATION ( #14983, #4652 ) ;
#10760 = CARTESIAN_POINT ( 'NONE',  ( 0.02436607992775544421, -22.71065055754445439, -9.836394144775947979 ) ) ;
#10761 = SURFACE_STYLE_FILL_AREA ( #18457 ) ;
#10762 = VERTEX_POINT ( 'NONE', #2014 ) ;
#10763 = VERTEX_POINT ( 'NONE', #6207 ) ;
#10764 = CARTESIAN_POINT ( 'NONE',  ( 4.476417968967386862, 17.43449690031536292, -35.00000000000000000 ) ) ;
#10765 = CARTESIAN_POINT ( 'NONE',  ( 2.604434325169353581, -2.851997810081467577, -25.77772010606609498 ) ) ;
#10766 = ORIENTED_EDGE ( 'NONE', *, *, #14108, .F. ) ;
#10767 = ADVANCED_FACE ( 'NONE', ( #9327, #9433 ), #8114, .T. ) ;
#10768 = ADVANCED_FACE ( 'NONE', ( #9231 ), #12333, .F. ) ;
#10769 = CARTESIAN_POINT ( 'NONE',  ( 2.000000000000001776, 5.908920805885978590E-16, 4.824999999999999289 ) ) ;
#10770 = ADVANCED_FACE ( 'NONE', ( #6396 ), #13944, .T. ) ;
#10771 = ORIENTED_EDGE ( 'NONE', *, *, #5279, .T. ) ;
#10772 = AXIS2_PLACEMENT_3D ( 'NONE', #2622, #5624, #11738 ) ;
#10773 = AXIS2_PLACEMENT_3D ( 'NONE', #1116, #7189, #6904 ) ;
#10774 = DIRECTION ( 'NONE',  ( 1.000000000000000000, 0.000000000000000000, 0.000000000000000000 ) ) ;
#10775 = FACE_OUTER_BOUND ( 'NONE', #19106, .T. ) ;
#10776 = CARTESIAN_POINT ( 'NONE',  ( -2.000000000000001776, -3.950217066951263956, -3.681818181818183877 ) ) ;
#10777 = ORIENTED_EDGE ( 'NONE', *, *, #8732, .T. ) ;
#10778 = ORIENTED_EDGE ( 'NONE', *, *, #18398, .T. ) ;
#10779 = DIRECTION ( 'NONE',  ( 0.000000000000000000, 1.776356839400250465E-15, 1.000000000000000000 ) ) ;
#10780 = CARTESIAN_POINT ( 'NONE',  ( 1.749999999999998002, 0.000000000000000000, 0.000000000000000000 ) ) ;
#10781 = VERTEX_POINT ( 'NONE', #316 ) ;
#10782 = AXIS2_PLACEMENT_3D ( 'NONE', #15129, #522, #18914 ) ;
#10783 = VERTEX_POINT ( 'NONE', #1912 ) ;
#10784 = DIRECTION ( 'NONE',  ( 0.000000000000000000, -1.000000000000000000, 0.000000000000000000 ) ) ;
#10785 = FACE_BOUND ( 'NONE', #5261, .T. ) ;
#10786 = DIRECTION ( 'NONE',  ( 0.000000000000000000, 0.000000000000000000, 1.000000000000000000 ) ) ;
#10787 = LINE ( 'NONE', #12485, #1352 ) ;
#10788 = CARTESIAN_POINT ( 'NONE',  ( -4.942249507334553371, 0.2590123213421660631, -10.34374999795161543 ) ) ;
#10789 = VECTOR ( 'NONE', #14159, 1000.000000000000000 ) ;
#10790 = VERTEX_POINT ( 'NONE', #12528 ) ;
#10791 = CARTESIAN_POINT ( 'NONE',  ( 6.843749997951615427, -4.233219804643852946, -2.444050593750049849 ) ) ;
#10792 = CARTESIAN_POINT ( 'NONE',  ( 16.19790265903627358, 9.644882309621939598, -32.00000000000000000 ) ) ;
#10793 = ORIENTED_EDGE ( 'NONE', *, *, #5543, .F. ) ;
#10794 = CARTESIAN_POINT ( 'NONE',  ( 11.50000000000000355, 3.631840208645857437, -4.484949146646330931 ) ) ;
#10795 = ADVANCED_FACE ( 'NONE', ( #9530 ), #418, .T. ) ;
#10796 = ADVANCED_FACE ( 'NONE', ( #12822 ), #4009, .F. ) ;
#10797 = DIRECTION ( 'NONE',  ( 0.000000000000000000, 0.000000000000000000, 1.000000000000000000 ) ) ;
#10798 = CARTESIAN_POINT ( 'NONE',  ( -2.000000000000001776, 3.950217066951266176, -3.681818181818181213 ) ) ;
#10799 = CARTESIAN_POINT ( 'NONE',  ( 0.000000000000000000, -24.04302995059965653, -1.991882183130557094 ) ) ;
#10800 = ORIENTED_EDGE ( 'NONE', *, *, #2231, .T. ) ;
#10801 = CIRCLE ( 'NONE', #15602, 24.12539914357697768 ) ;
#10802 = CARTESIAN_POINT ( 'NONE',  ( 13.96874999795161365, 3.499494075959816541, 3.499494075959815653 ) ) ;
#10803 =( LENGTH_UNIT ( ) NAMED_UNIT ( * ) SI_UNIT ( .MILLI., .METRE. ) );
#10804 = FACE_OUTER_BOUND ( 'NONE', #7040, .T. ) ;
#10805 = VECTOR ( 'NONE', #11920, 1000.000000000000000 ) ;
#10806 = EDGE_CURVE ( 'NONE', #19214, #9684, #7083, .T. ) ;
#10807 = FACE_OUTER_BOUND ( 'NONE', #8655, .T. ) ;
#10808 = ORIENTED_EDGE ( 'NONE', *, *, #8852, .F. ) ;
#10809 = FACE_OUTER_BOUND ( 'NONE', #15863, .T. ) ;
#10810 = DIRECTION ( 'NONE',  ( -1.000000000000000000, -0.000000000000000000, -0.000000000000000000 ) ) ;
#10811 = CARTESIAN_POINT ( 'NONE',  ( 13.00000000000000533, -0.5958122406256377568, 5.668774803599156975 ) ) ;
#10812 = CARTESIAN_POINT ( 'NONE',  ( 0.0003207540509378258692, 20.70663861606293921, -12.51925356660738053 ) ) ;
#10813 = ORIENTED_EDGE ( 'NONE', *, *, #4065, .F. ) ;
#10814 = CARTESIAN_POINT ( 'NONE',  ( 0.1855654851361735469, 10.67816411292198175, -23.63475234378971379 ) ) ;
#10815 = ADVANCED_FACE ( 'NONE', ( #11220 ), #18723, .T. ) ;
#10816 = CARTESIAN_POINT ( 'NONE',  ( 4.233219804643887585, 2.444050593749991229, -11.84374999795161365 ) ) ;
#10817 = EDGE_CURVE ( 'NONE', #19442, #12550, #19679, .T. ) ;
#10818 = ORIENTED_EDGE ( 'NONE', *, *, #13741, .T. ) ;
#10819 = CARTESIAN_POINT ( 'NONE',  ( 2.789999999999999147, -20.62201879784921843, 12.52067188844344336 ) ) ;
#10820 = AXIS2_PLACEMENT_3D ( 'NONE', #3969, #13074, #6653 ) ;
#10821 = VERTEX_POINT ( 'NONE', #8314 ) ;
#10822 = CONTEXT_DEPENDENT_SHAPE_REPRESENTATION ( #9367, #14665 ) ;
#10823 = CARTESIAN_POINT ( 'NONE',  ( 1.039999999999998925, -4.147968289691484678, 27.76164181293050248 ) ) ;
#10824 = CARTESIAN_POINT ( 'NONE',  ( 0.02436607992776498519, 9.836394144775706394, 22.71065055754456097 ) ) ;
#10825 = EDGE_LOOP ( 'NONE', ( #3668, #926 ) ) ;
#10826 = DIRECTION ( 'NONE',  ( 0.000000000000000000, 0.000000000000000000, 1.000000000000000000 ) ) ;
#10827 = DIRECTION ( 'NONE',  ( -0.000000000000000000, -0.000000000000000000, -1.000000000000000000 ) ) ;
#10828 = EDGE_CURVE ( 'NONE', #11862, #13666, #17322, .T. ) ;
#10829 = ORIENTED_EDGE ( 'NONE', *, *, #3310, .F. ) ;
#10830 = DIRECTION ( 'NONE',  ( 0.000000000000000000, 0.000000000000000000, 1.000000000000000000 ) ) ;
#10831 = ORIENTED_EDGE ( 'NONE', *, *, #4899, .T. ) ;
#10833 = DIRECTION ( 'NONE',  ( 0.000000000000000000, -1.000000000000000000, 0.000000000000000000 ) ) ;
#10832 = VECTOR ( 'NONE', #17210, 1000.000000000000114 ) ;
#10834 = ORIENTED_EDGE ( 'NONE', *, *, #5982, .T. ) ;
#10835 = DIRECTION ( 'NONE',  ( 0.000000000000000000, 0.000000000000000000, -1.000000000000000000 ) ) ;
#10836 = CARTESIAN_POINT ( 'NONE',  ( 2.444050593749960587, -4.233219804643904460, -6.843749997951615427 ) ) ;
#10837 = CARTESIAN_POINT ( 'NONE',  ( -4.840010801796527318, -3.143139765844555900, -7.500000000000005329 ) ) ;
#10838 = EDGE_CURVE ( 'NONE', #16718, #19487, #11611, .T. ) ;
#10839 = CARTESIAN_POINT ( 'NONE',  ( 13.00000000000000000, 0.2080849974989116558, 4.883670121236158401 ) ) ;
#10840 = AXIS2_PLACEMENT_3D ( 'NONE', #4157, #8959, #8863 ) ;
#10841 = ADVANCED_FACE ( 'NONE', ( #12921, #19114 ), #8421, .T. ) ;
#10842 = VERTEX_POINT ( 'NONE', #19019 ) ;
#10843 = CARTESIAN_POINT ( 'NONE',  ( 2.790000000000076419, -20.85287692521938752, 12.51293083811791718 ) ) ;
#10844 = CYLINDRICAL_SURFACE ( 'NONE', #3672, 1.000000000000000888 ) ;
#10845 = AXIS2_PLACEMENT_3D ( 'NONE', #18567, #17267, #1767 ) ;
#10846 = ORIENTED_EDGE ( 'NONE', *, *, #19070, .F. ) ;
#10847 = EDGE_CURVE ( 'NONE', #14373, #11454, #9473, .T. ) ;
#10848 = CARTESIAN_POINT ( 'NONE',  ( -19.00000000000000355, 3.434748899119118626, 2.750000000000001776 ) ) ;
#10849 = DIRECTION ( 'NONE',  ( -0.000000000000000000, -0.000000000000000000, 1.000000000000000000 ) ) ;
#10850 = ORIENTED_EDGE ( 'NONE', *, *, #12607, .T. ) ;
#10852 = FACE_OUTER_BOUND ( 'NONE', #10375, .T. ) ;
#10851 = CIRCLE ( 'NONE', #18208, 5.700000000000001954 ) ;
#10853 = CARTESIAN_POINT ( 'NONE',  ( 7.812499995903224637, -4.484949146646330931, -3.631840208645857437 ) ) ;
#10854 = ORIENTED_EDGE ( 'NONE', *, *, #16653, .F. ) ;
#10855 = CARTESIAN_POINT ( 'NONE',  ( 2.789999999999999147, 20.62201879784912606, 12.52067188844359080 ) ) ;
#10856 = VERTEX_POINT ( 'NONE', #14716 ) ;
#10857 = SHAPE_DEFINITION_REPRESENTATION ( #12735, #18211 ) ;
#10858 = CARTESIAN_POINT ( 'NONE',  ( -2.318398865532109721, -5.207209108562803834, -9.000000000000005329 ) ) ;
#10859 = DIRECTION ( 'NONE',  ( 0.000000000000000000, 0.000000000000000000, 1.000000000000000000 ) ) ;
#10860 = EDGE_LOOP ( 'NONE', ( #16527, #3349, #10062, #16876, #11226, #2055, #13016, #12381 ) ) ;
#10861 = ORIENTED_EDGE ( 'NONE', *, *, #3515, .F. ) ;
#10862 = CARTESIAN_POINT ( 'NONE',  ( 0.07181524296601660140, -16.91181672897718968, -18.89296398180210446 ) ) ;
#10863 = CARTESIAN_POINT ( 'NONE',  ( 2.765633920072239516, -2.336989772644097574, -24.63872515616085224 ) ) ;
#10864 = EDGE_CURVE ( 'NONE', #19421, #9729, #12350, .T. ) ;
#10865 = ORIENTED_EDGE ( 'NONE', *, *, #16653, .T. ) ;
#10866 = TOROIDAL_SURFACE ( 'NONE', #13410, 24.12539914357697768, 8.000000000000000000 ) ;
#10867 = CARTESIAN_POINT ( 'NONE',  ( 17.68117051311639898, -3.372863662543048591, -32.00000000000000000 ) ) ;
#10868 = ORIENTED_EDGE ( 'NONE', *, *, #18375, .T. ) ;
#10869 = FACE_OUTER_BOUND ( 'NONE', #4261, .T. ) ;
#10870 = CARTESIAN_POINT ( 'NONE',  ( 2.000000000000000000, -2.000000000000001776, 37.99999999999999289 ) ) ;
#10871 = DIRECTION ( 'NONE',  ( 0.000000000000000000, 0.000000000000000000, 1.000000000000000000 ) ) ;
#10872 = EDGE_CURVE ( 'NONE', #18625, #5897, #14424, .T. ) ;
#10873 = CARTESIAN_POINT ( 'NONE',  ( 2.262072637928882468, -12.96450951081233605, 23.73240184472491876 ) ) ;
#10874 = ORIENTED_EDGE ( 'NONE', *, *, #8690, .F. ) ;
#10875 = AXIS2_PLACEMENT_3D ( 'NONE', #181, #16801, #10786 ) ;
#10876 = ORIENTED_EDGE ( 'NONE', *, *, #8826, .F. ) ;
#10877 = CARTESIAN_POINT ( 'NONE',  ( 1.749999999999998002, -20.02152543075360214, 19.67366047555523068 ) ) ;
#10878 =( NAMED_UNIT ( * ) SI_UNIT ( $, .STERADIAN. ) SOLID_ANGLE_UNIT ( ) );
#10879 = AXIS2_PLACEMENT_3D ( 'NONE', #13220, #15113, #8708 ) ;
#10880 = DIRECTION ( 'NONE',  ( -1.000000000000000000, -0.000000000000000000, -0.000000000000000000 ) ) ;
#10881 = ORIENTED_EDGE ( 'NONE', *, *, #18771, .T. ) ;
#10882 = ORIENTED_EDGE ( 'NONE', *, *, #18987, .T. ) ;
#10883 = CARTESIAN_POINT ( 'NONE',  ( 0.000000000000000000, 0.000000000000000000, -29.00000000000000000 ) ) ;
#10884 = CARTESIAN_POINT ( 'NONE',  ( -5.575441324182703440, -1.185096637661177343, -13.31249999590322730 ) ) ;
#10885 = DIRECTION ( 'NONE',  ( 1.000000000000000000, 0.000000000000000000, 0.000000000000000000 ) ) ;
#10886 = EDGE_CURVE ( 'NONE', #1540, #17520, #5211, .T. ) ;
#10887 = CARTESIAN_POINT ( 'NONE',  ( 2.724374482943360487, 21.84204283372364230, 12.72258903105646688 ) ) ;
#10888 = CARTESIAN_POINT ( 'NONE',  ( -4.888101187500000222, 0.000000000000000000, -6.468749997951615427 ) ) ;
#10889 = VERTEX_POINT ( 'NONE', #16019 ) ;
#10890 = CARTESIAN_POINT ( 'NONE',  ( 7.626241948324204323, -16.73597674598852691, 35.00000000000000000 ) ) ;
#10891 = CARTESIAN_POINT ( 'NONE',  ( 15.19790265903627358, 9.644882309621939598, -32.00000000000000000 ) ) ;
#10892 = VECTOR ( 'NONE', #18302, 1000.000000000000000 ) ;
#10893 = ORIENTED_EDGE ( 'NONE', *, *, #8457, .T. ) ;
#10894 = CARTESIAN_POINT ( 'NONE',  ( 7.000000000000005329, -3.814044456245443193, -4.235925505221191933 ) ) ;
#10895 = CIRCLE ( 'NONE', #5759, 1.000000000000002442 ) ;
#10896 = CYLINDRICAL_SURFACE ( 'NONE', #14733, 6.000000000000021316 ) ;
#10897 = DIRECTION ( 'NONE',  ( -0.000000000000000000, -0.000000000000000000, 1.000000000000000000 ) ) ;
#10898 = ADVANCED_FACE ( 'NONE', ( #16130 ), #16185, .T. ) ;
#10899 = PRODUCT_DEFINITION ( 'UNKNOWN', '', #10200, #13587 ) ;
#10900 = VERTEX_POINT ( 'NONE', #16220 ) ;
#10901 = CARTESIAN_POINT ( 'NONE',  ( 0.1882238782932344201, 17.47009390565490605, 19.18368891937496556 ) ) ;
#10902 = CARTESIAN_POINT ( 'NONE',  ( -10.00000000000000000, 0.000000000000000000, 0.000000000000000000 ) ) ;
#10903 = ORIENTED_EDGE ( 'NONE', *, *, #13821, .F. ) ;
#10904 =( BOUNDED_CURVE ( )  B_SPLINE_CURVE ( 2, ( #299, #12610, #4995, #8500, #17597, #10102, #16202, #2384, #2476, #9913, #10007, #6677, #8398 ),
 .UNSPECIFIED., .F., .F. ) 
 B_SPLINE_CURVE_WITH_KNOTS ( ( 3, 2, 2, 2, 2, 2, 3 ),
 ( 0.000000000000000000, 0.05000000000000000278, 0.1000000000000000056, 0.1499999999999999944, 0.2000000000000000111, 0.2500000000000000000, 0.2843253191101273170 ),
 .UNSPECIFIED. ) 
 CURVE ( )  GEOMETRIC_REPRESENTATION_ITEM ( )  RATIONAL_B_SPLINE_CURVE ( ( 1.000000000000000000, 0.9876883405951377704, 1.000000000000000000, 0.9876883405951377704, 1.000000000000000000, 0.9876883405951377704, 1.000000000000000000, 0.9876883405951377704, 1.000000000000000000, 0.9876883405951377704, 1.000000000000000000, 0.9915479672430580482, 0.9947006833465674713 ) ) 
 REPRESENTATION_ITEM ( '' )  );
#10905 = DIRECTION ( 'NONE',  ( 0.000000000000000000, -8.881784197001252323E-16, 1.000000000000000000 ) ) ;
#10906 = AXIS2_PLACEMENT_3D ( 'NONE', #12841, #337, #3440 ) ;
#10907 = DIRECTION ( 'NONE',  ( 0.9238795325112864054, 0.3826834323650906700, 0.000000000000000000 ) ) ;
#10908 = EDGE_CURVE ( 'NONE', #12853, #16351, #15583, .T. ) ;
#10909 = AXIS2_PLACEMENT_3D ( 'NONE', #12243, #5924, #4338 ) ;
#10910 = CARTESIAN_POINT ( 'NONE',  ( 13.00000000000000178, -3.849641071994423402, 3.458892414715191599 ) ) ;
#10911 = EDGE_LOOP ( 'NONE', ( #11243, #5255 ) ) ;
#10912 = ADVANCED_FACE ( 'NONE', ( #3810 ), #7526, .T. ) ;
#10913 = DIRECTION ( 'NONE',  ( -0.000000000000000000, -0.000000000000000000, -1.000000000000000000 ) ) ;
#10914 = DIRECTION ( 'NONE',  ( 0.000000000000000000, 0.000000000000000000, 1.000000000000000000 ) ) ;
#10915 = ORIENTED_EDGE ( 'NONE', *, *, #13709, .T. ) ;
#10916 = CARTESIAN_POINT ( 'NONE',  ( 6.000000000000005329, -4.936344801571268093, -2.850000000000058265 ) ) ;
#10917 = CARTESIAN_POINT ( 'NONE',  ( 0.5321745087963422050, -11.58891744060090367, -24.44564404695856297 ) ) ;
#10918 = ORIENTED_EDGE ( 'NONE', *, *, #4191, .F. ) ;
#10919 = EDGE_CURVE ( 'NONE', #7633, #15498, #17772, .T. ) ;
#10920 = AXIS2_PLACEMENT_3D ( 'NONE', #18099, #4389, #2879 ) ;
#10921 = CIRCLE ( 'NONE', #7727, 1.000000000000003109 ) ;
#10922 = LINE ( 'NONE', #11119, #12837 ) ;
#10923 = CARTESIAN_POINT ( 'NONE',  ( 5.700000000000001066, -3.980288726281172656E-14, -7.312499995903225525 ) ) ;
#10924 = VERTEX_POINT ( 'NONE', #6992 ) ;
#10925 = CARTESIAN_POINT ( 'NONE',  ( 0.006974771092478231072, 9.686319561460942751, 22.53337530003406997 ) ) ;
#10927 = ADVANCED_FACE ( 'NONE', ( #16609 ), #12109, .T. ) ;
#10926 = ADVANCED_FACE ( 'NONE', ( #5501, #8705 ), #2891, .T. ) ;
#10928 = CYLINDRICAL_SURFACE ( 'NONE', #9422, 14.00000000000000178 ) ;
#10929 = ORIENTED_EDGE ( 'NONE', *, *, #13205, .F. ) ;
#10930 = CARTESIAN_POINT ( 'NONE',  ( -11.00000000000000355, -5.400000000000001243, 0.000000000000000000 ) ) ;
#10931 = ORIENTED_EDGE ( 'NONE', *, *, #3929, .T. ) ;
#10932 = CARTESIAN_POINT ( 'NONE',  ( 2.765633920072242624, -22.71065055754459650, 9.836394144775621129 ) ) ;
#10933 = ORIENTED_EDGE ( 'NONE', *, *, #17138, .T. ) ;
#10934 = DIRECTION ( 'NONE',  ( 0.000000000000000000, 0.000000000000000000, 1.000000000000000000 ) ) ;
#10935 = DIRECTION ( 'NONE',  ( 1.000000000000000000, 0.000000000000000000, 0.000000000000000000 ) ) ;
#10936 = DIRECTION ( 'NONE',  ( 0.000000000000000000, 0.000000000000000000, 1.000000000000000000 ) ) ;
#10937 = AXIS2_PLACEMENT_3D ( 'NONE', #3981, #885, #2468 ) ;
#10938 = VECTOR ( 'NONE', #13673, 1000.000000000000000 ) ;
#10939 = CARTESIAN_POINT ( 'NONE',  ( 3.270778111535314281, -3.632567103900546712, -12.46874999795161543 ) ) ;
#10940 = VERTEX_POINT ( 'NONE', #16414 ) ;
#10941 = AXIS2_PLACEMENT_3D ( 'NONE', #6358, #3380, #10592 ) ;
#10942 = FACE_BOUND ( 'NONE', #19335, .T. ) ;
#10943 = CARTESIAN_POINT ( 'NONE',  ( 0.02436607992776151574, -16.37294372382871188, 18.55949924794887096 ) ) ;
#10944 = VECTOR ( 'NONE', #8497, 1000.000000000000000 ) ;
#10945 = EDGE_LOOP ( 'NONE', ( #7223, #9307, #17575, #6089 ) ) ;
#10946 = CARTESIAN_POINT ( 'NONE',  ( -2.000000000000001776, 0.000000000000000000, 0.000000000000000000 ) ) ;
#10947 = DIRECTION ( 'NONE',  ( 0.000000000000000000, 1.000000000000000000, 0.000000000000000000 ) ) ;
#10948 = VERTEX_POINT ( 'NONE', #19303 ) ;
#10949 = CIRCLE ( 'NONE', #9035, 6.200000000000020606 ) ;
#10950 = DIRECTION ( 'NONE',  ( 1.000000000000000000, 0.000000000000000000, 0.000000000000000000 ) ) ;
#10951 = COLOUR_RGB ( '', 0.08235294, 0.09019608, 0.10196078) ;
#10952 = CARTESIAN_POINT ( 'NONE',  ( 9.843749997951615427, -0.5109457054261099529, -4.861323657744413218 ) ) ;
#10953 = VECTOR ( 'NONE', #15784, 1000.000000000000114 ) ;
#10954 = ORIENTED_EDGE ( 'NONE', *, *, #9669, .F. ) ;
#10955 = CARTESIAN_POINT ( 'NONE',  ( 2.500000000000002220, 9.887492094615969966E-16, 8.073750000000021743 ) ) ;
#10956 = ORIENTED_EDGE ( 'NONE', *, *, #197, .T. ) ;
#10957 = VECTOR ( 'NONE', #11145, 1000.000000000000000 ) ;
#10958 = APPLICATION_PROTOCOL_DEFINITION ( 'draft international standard', 'automotive_design', 1998, #9843 ) ;
#10959 = CARTESIAN_POINT ( 'NONE',  ( 0.3020334839682081163, -5.763142191869158992, -7.500000000000005329 ) ) ;
#10960 = CARTESIAN_POINT ( 'NONE',  ( 11.84374999795161365, 2.444050593749990785, 4.233219804643887585 ) ) ;
#10961 = CIRCLE ( 'NONE', #4884, 4.762499999999999289 ) ;
#10962 = VERTEX_POINT ( 'NONE', #2691 ) ;
#10963 = ORIENTED_EDGE ( 'NONE', *, *, #51, .F. ) ;
#10964 = CARTESIAN_POINT ( 'NONE',  ( 1.039999999999998259, 12.52377138324223615, 25.12109765559657859 ) ) ;
#10965 = CARTESIAN_POINT ( 'NONE',  ( -19.00000000000000355, -4.400000000000000355, 5.388445916248354013E-16 ) ) ;
#10966 = ORIENTED_EDGE ( 'NONE', *, *, #17243, .T. ) ;
#10967 = AXIS2_PLACEMENT_3D ( 'NONE', #18868, #5152, #11271 ) ;
#10968 = DIRECTION ( 'NONE',  ( 1.000000000000000000, 0.000000000000000000, 0.000000000000000000 ) ) ;
#10969 = ORIENTED_EDGE ( 'NONE', *, *, #840, .F. ) ;
#10970 = VECTOR ( 'NONE', #11632, 1000.000000000000000 ) ;
#10971 = AXIS2_PLACEMENT_3D ( 'NONE', #1799, #4996, #4800 ) ;
#10972 = CARTESIAN_POINT ( 'NONE',  ( -5.700000000000001066, -0.5990941410143296730, -12.33180101230370518 ) ) ;
#10973 = ADVANCED_FACE ( 'NONE', ( #19703 ), #5893, .F. ) ;
#10974 = CARTESIAN_POINT ( 'NONE',  ( 0.006974771092478813939, -22.53337530003410905, 9.686319561460866367 ) ) ;
#10975 = FACE_BOUND ( 'NONE', #14238, .T. ) ;
#10976 = ORIENTED_EDGE ( 'NONE', *, *, #456, .F. ) ;
#10977 = CARTESIAN_POINT ( 'NONE',  ( -15.00000000000000355, 3.434748899119118182, -2.750000000000002665 ) ) ;
#10978 = CARTESIAN_POINT ( 'NONE',  ( -16.28688694438836038, -7.664027248171298545, 32.00000000000000000 ) ) ;
#10979 = VERTEX_POINT ( 'NONE', #7486 ) ;
#10980 = EDGE_LOOP ( 'NONE', ( #12713, #8937, #3951, #13344 ) ) ;
#10981 = CARTESIAN_POINT ( 'NONE',  ( 0.000000000000000000, -20.62201879784923264, 12.52067188844344336 ) ) ;
#10982 = LINE ( 'NONE', #7965, #7339 ) ;
#10983 = CONICAL_SURFACE ( 'NONE', #14179, 4.000000000000000000, 0.2132412839022289897 ) ;
#10984 = CARTESIAN_POINT ( 'NONE',  ( -18.96448111170889206, 1.130229351527647808, 32.00000000000000000 ) ) ;
#10985 = CARTESIAN_POINT ( 'NONE',  ( -2.873153789725825469, 3.954556930911862000, -9.468749997951615427 ) ) ;
#10986 = ORIENTED_EDGE ( 'NONE', *, *, #11742, .T. ) ;
#10987 = CARTESIAN_POINT ( 'NONE',  ( 0.000000000000000000, 18.28042085475300382, -15.74360496233363804 ) ) ;
#10988 = EDGE_CURVE ( 'NONE', #13429, #10783, #8808, .T. ) ;
#10989 = CARTESIAN_POINT ( 'NONE',  ( 8.843749997951615427, -2.873153789725853002, 3.954556930911842016 ) ) ;
#10990 =( GEOMETRIC_REPRESENTATION_CONTEXT ( 3 ) GLOBAL_UNCERTAINTY_ASSIGNED_CONTEXT ( ( #13197 ) ) GLOBAL_UNIT_ASSIGNED_CONTEXT ( ( #14070, #268, #10878 ) ) REPRESENTATION_CONTEXT ( 'NONE', 'WORKASPACE' ) );
#10991 = VERTEX_POINT ( 'NONE', #4400 ) ;
#10992 = CARTESIAN_POINT ( 'NONE',  ( 14.46874999795161720, 4.861323657744413218, -0.5109457054261112852 ) ) ;
#10993 = CARTESIAN_POINT ( 'NONE',  ( 12.84374999795161543, -1.016293382781378485, -4.781284448697201483 ) ) ;
#10994 = EDGE_CURVE ( 'NONE', #6503, #4959, #14814, .T. ) ;
#10995 = CYLINDRICAL_SURFACE ( 'NONE', #388, 0.9999999999999974465 ) ;
#10996 = CYLINDRICAL_SURFACE ( 'NONE', #116, 2.524999999999995914 ) ;
#10997 = CARTESIAN_POINT ( 'NONE',  ( 4.888101187500000222, -3.413342815706642518E-14, -6.468749997951615427 ) ) ;
#10998 = ORIENTED_EDGE ( 'NONE', *, *, #10093, .F. ) ;
#10999 = DIRECTION ( 'NONE',  ( 1.000000000000000000, 0.000000000000000000, 0.000000000000000000 ) ) ;
#11000 = DIRECTION ( 'NONE',  ( -0.000000000000000000, -0.000000000000000000, 1.000000000000000000 ) ) ;
#11001 = FACE_OUTER_BOUND ( 'NONE', #2882, .T. ) ;
#11002 = ORIENTED_EDGE ( 'NONE', *, *, #4599, .T. ) ;
#11003 = CARTESIAN_POINT ( 'NONE',  ( -15.28688694438835505, -7.664027248171298545, -32.00000000000000000 ) ) ;
#11004 = AXIS2_PLACEMENT_3D ( 'NONE', #11451, #2525, #7018 ) ;
#11005 = CARTESIAN_POINT ( 'NONE',  ( 6.468749997951615427, -4.233219804643852946, -2.444050593750049849 ) ) ;
#11006 = DIRECTION ( 'NONE',  ( 1.000000000000000000, 0.000000000000000000, 0.000000000000000000 ) ) ;
#11007 = VERTEX_POINT ( 'NONE', #13217 ) ;
#11008 = CARTESIAN_POINT ( 'NONE',  ( 2.765633920072233742, -24.15498966839966855, 5.391175441198523544 ) ) ;
#11009 = CARTESIAN_POINT ( 'NONE',  ( -2.993098736590125853E-16, 4.888101187500000222, -11.84374999795161365 ) ) ;
#11010 = EDGE_LOOP ( 'NONE', ( #15983, #6585, #6620, #10538 ) ) ;
#11011 = AXIS2_PLACEMENT_3D ( 'NONE', #18918, #3322, #9434 ) ;
#11012 = CARTESIAN_POINT ( 'NONE',  ( 8.343749997951611874, -2.246813503491864150, 4.409619785863891472 ) ) ;
#11013 = EDGE_CURVE ( 'NONE', #6013, #12765, #18112, .T. ) ;
#11014 = CARTESIAN_POINT ( 'NONE',  ( 1.039999999999997149, -4.633866840648735774, -27.68468304288263226 ) ) ;
#11015 = EDGE_CURVE ( 'NONE', #271, #10979, #219, .T. ) ;
#11016 = VERTEX_POINT ( 'NONE', #13606 ) ;
#11017 = ITEM_DEFINED_TRANSFORMATION ( 'NONE', 'NONE', #6345,  #16724 ) ;
#11018 = EDGE_CURVE ( 'NONE', #12265, #9627, #4839, .T. ) ;
#11019 = STYLED_ITEM ( 'NONE', ( #13647 ), #9397 ) ;
#11020 = CARTESIAN_POINT ( 'NONE',  ( 1.749999999999998002, 19.67366047555530528, 20.02152543075352753 ) ) ;
#11021 = DIRECTION ( 'NONE',  ( -0.9773501006361904331, 2.591706245282795403E-17, -0.2116288751244229938 ) ) ;
#11022 =( BOUNDED_CURVE ( )  B_SPLINE_CURVE ( 2, ( #6684, #3203, #15418, #14013, #1714, #7802, #18512, #306, #12516, #18609, #11009, #9520, #15615, #14107, #17701, #3894, #707 ),
 .UNSPECIFIED., .F., .F. ) 
 B_SPLINE_CURVE_WITH_KNOTS ( ( 3, 2, 2, 2, 2, 2, 2, 2, 3 ),
 ( 0.000000000000000000, 0.05000000000000000971, 0.1000000000000000194, 0.1499999999999999944, 0.2000000000000000389, 0.2500000000000000000, 0.2999999999999999889, 0.3499999999999999223, 0.4000000000000000777 ),
 .UNSPECIFIED. ) 
 CURVE ( )  GEOMETRIC_REPRESENTATION_ITEM ( )  RATIONAL_B_SPLINE_CURVE ( ( 1.000000000000000000, 0.9876883405951377704, 1.000000000000000000, 0.9876883405951377704, 1.000000000000000000, 0.9876883405951377704, 1.000000000000000000, 0.9876883405951377704, 1.000000000000000000, 0.9876883405951377704, 1.000000000000000000, 0.9876883405951377704, 1.000000000000000000, 0.9876883405951377704, 1.000000000000000000, 0.9876883405951377704, 1.000000000000000000 ) ) 
 REPRESENTATION_ITEM ( '' )  );
#11023 = ADVANCED_FACE ( 'NONE', ( #17813 ), #2762, .T. ) ;
#11024 = ORIENTED_EDGE ( 'NONE', *, *, #15251, .F. ) ;
#11025 = CARTESIAN_POINT ( 'NONE',  ( 1.749999999999998002, -27.76164181293049182, -4.147968289691579713 ) ) ;
#11026 = DIRECTION ( 'NONE',  ( -1.000000000000000000, -0.000000000000000000, -0.000000000000000000 ) ) ;
#11027 = ORIENTED_EDGE ( 'NONE', *, *, #10679, .F. ) ;
#11028 = CARTESIAN_POINT ( 'NONE',  ( 5.476417968967387750, 17.43449690031536292, 32.00000000000000000 ) ) ;
#11029 = ORIENTED_EDGE ( 'NONE', *, *, #3900, .T. ) ;
#11030 = LINE ( 'NONE', #9535, #880 ) ;
#11031 = ORIENTED_EDGE ( 'NONE', *, *, #9558, .T. ) ;
#11032 = CARTESIAN_POINT ( 'NONE',  ( -4.476417968967385974, 17.43449690031536292, -32.00000000000000000 ) ) ;
#11033 = DIRECTION ( 'NONE',  ( 0.000000000000000000, 0.000000000000000000, -1.000000000000000000 ) ) ;
#11034 = EDGE_CURVE ( 'NONE', #19646, #17299, #18019, .T. ) ;
#11035 = FACE_OUTER_BOUND ( 'NONE', #10101, .T. ) ;
#11036 = CARTESIAN_POINT ( 'NONE',  ( 3.270778111535314281, -3.632567103900546712, -12.84374999795161543 ) ) ;
#11037 = VECTOR ( 'NONE', #13679, 1000.000000000000000 ) ;
#11038 = EDGE_LOOP ( 'NONE', ( #11705, #1070, #6857, #9973, #18463, #15519 ) ) ;
#11039 = DIRECTION ( 'NONE',  ( 0.000000000000000000, 0.000000000000000000, 1.000000000000000000 ) ) ;
#11040 = CARTESIAN_POINT ( 'NONE',  ( 2.783068888626318405, 9.685942809247050533, 22.53293026234507579 ) ) ;
#11041 = ORIENTED_EDGE ( 'NONE', *, *, #13948, .T. ) ;
#11042 = EDGE_CURVE ( 'NONE', #4945, #1219, #3732, .T. ) ;
#11043 = EDGE_LOOP ( 'NONE', ( #11854, #10986, #1465, #13194 ) ) ;
#11044 = DIRECTION ( 'NONE',  ( 0.000000000000000000, 0.000000000000000000, -1.000000000000000000 ) ) ;
#11045 = LINE ( 'NONE', #18544, #5518 ) ;
#11046 = ORIENTED_EDGE ( 'NONE', *, *, #2897, .F. ) ;
#11047 = CARTESIAN_POINT ( 'NONE',  ( 2.500000000000000888, 7.592810154713616459E-16, 6.200000000000021494 ) ) ;
#11048 = CARTESIAN_POINT ( 'NONE',  ( 8.812499995903225525, -3.143139765844555900, -4.840010801796527318 ) ) ;
#11049 = AXIS2_PLACEMENT_3D ( 'NONE', #10279, #14975, #1367 ) ;
#11050 = ORIENTED_EDGE ( 'NONE', *, *, #13494, .F. ) ;
#11051 = CARTESIAN_POINT ( 'NONE',  ( 2.000000000000001776, 0.000000000000000000, 0.000000000000000000 ) ) ;
#11052 = VERTEX_POINT ( 'NONE', #1109 ) ;
#11053 = APPLICATION_PROTOCOL_DEFINITION ( 'draft international standard', 'automotive_design', 1998, #11487 ) ;
#11054 = CARTESIAN_POINT ( 'NONE',  ( -4.936344801571327601, -2.849999999999954792, -11.00000000000000711 ) ) ;
#11055 = FACE_OUTER_BOUND ( 'NONE', #11460, .T. ) ;
#11056 = ADVANCED_FACE ( 'NONE', ( #4302 ), #13069, .F. ) ;
#11057 = ORIENTED_EDGE ( 'NONE', *, *, #9093, .T. ) ;
#11058 = ORIENTED_EDGE ( 'NONE', *, *, #14767, .F. ) ;
#11059 = CYLINDRICAL_SURFACE ( 'NONE', #16261, 4.762500000000000178 ) ;
#11060 = CARTESIAN_POINT ( 'NONE',  ( 1.039999999999997593, 0.000000000000000000, 0.000000000000000000 ) ) ;
#11061 = ORIENTED_EDGE ( 'NONE', *, *, #5890, .T. ) ;
#11062 = EDGE_CURVE ( 'NONE', #1448, #5844, #7874, .T. ) ;
#11063 = AXIS2_PLACEMENT_3D ( 'NONE', #13113, #6894, #5104 ) ;
#11064 = EDGE_CURVE ( 'NONE', #6948, #5629, #14915, .T. ) ;
#11065 = AXIS2_PLACEMENT_3D ( 'NONE', #18229, #114, #12125 ) ;
#11066 = CARTESIAN_POINT ( 'NONE',  ( -22.50000000000000711, -21.04737509655562988, 0.000000000000000000 ) ) ;
#11067 = ORIENTED_EDGE ( 'NONE', *, *, #15941, .F. ) ;
#11068 = CARTESIAN_POINT ( 'NONE',  ( 12.46874999795161543, -1.016293382781378485, -4.781284448697201483 ) ) ;
#11069 = DIRECTION ( 'NONE',  ( 1.000000000000000000, 0.000000000000000000, 0.000000000000000000 ) ) ;
#11070 = DIRECTION ( 'NONE',  ( -0.000000000000000000, -0.000000000000000000, 1.000000000000000000 ) ) ;
#11071 = AXIS2_PLACEMENT_3D ( 'NONE', #5286, #13090, #1988 ) ;
#11072 = ORIENTED_EDGE ( 'NONE', *, *, #11189, .T. ) ;
#11073 = DIRECTION ( 'NONE',  ( 0.000000000000000000, 0.000000000000000000, 1.000000000000000000 ) ) ;
#11074 =( LENGTH_UNIT ( ) NAMED_UNIT ( * ) SI_UNIT ( .MILLI., .METRE. ) );
#11075 = CARTESIAN_POINT ( 'NONE',  ( 6.000000000000005329, -4.936344801571268093, -2.850000000000058265 ) ) ;
#11076 = AXIS2_PLACEMENT_3D ( 'NONE', #18783, #588, #5074 ) ;
#11077 = EDGE_CURVE ( 'NONE', #17840, #720, #12501, .T. ) ;
#11078 = EDGE_LOOP ( 'NONE', ( #18572, #10123, #18677, #10634 ) ) ;
#11079 = ORIENTED_EDGE ( 'NONE', *, *, #7818, .T. ) ;
#11080 = CARTESIAN_POINT ( 'NONE',  ( 0.000000000000000000, 15.04425356660790136, -20.70663861606255196 ) ) ;
#11081 = CARTESIAN_POINT ( 'NONE',  ( 9.580134541264516912, -14.56230589874905412, -35.00000000000000000 ) ) ;
#11082 = CARTESIAN_POINT ( 'NONE',  ( -2.993098736590125853E-16, 4.888101187500000222, -11.46874999795161543 ) ) ;
#11083 = ADVANCED_FACE ( 'NONE', ( #15697 ), #15603, .F. ) ;
#11084 = EDGE_LOOP ( 'NONE', ( #10456, #11169, #11377, #19330 ) ) ;
#11085 = CARTESIAN_POINT ( 'NONE',  ( -90.00000000000000000, 9.887492094615969966E-16, 8.073750000000021743 ) ) ;
#11086 = CARTESIAN_POINT ( 'NONE',  ( -17.11901729331276911, 5.562305898749051458, -35.00000000000000000 ) ) ;
#11087 = CIRCLE ( 'NONE', #17487, 4.200000000000001954 ) ;
#11088 = ORIENTED_EDGE ( 'NONE', *, *, #6861, .T. ) ;
#11089 = DIRECTION ( 'NONE',  ( -0.000000000000000000, -0.000000000000000000, -1.000000000000000000 ) ) ;
#11090 = CIRCLE ( 'NONE', #10138, 28.06981291497571362 ) ;
#11091 = FACE_OUTER_BOUND ( 'NONE', #342, .T. ) ;
#11092 = ADVANCED_FACE ( 'NONE', ( #8604 ), #6085, .F. ) ;
#11093 = DIRECTION ( 'NONE',  ( 1.000000000000000000, 0.000000000000000000, 0.000000000000000000 ) ) ;
#11094 = CARTESIAN_POINT ( 'NONE',  ( 0.02436607992776325046, -24.15498966839958683, -5.391175441198872598 ) ) ;
#11095 = CARTESIAN_POINT ( 'NONE',  ( 4.080749450109621534, -4.080749450109678378, -8.500000000000007105 ) ) ;
#11096 = VERTEX_POINT ( 'NONE', #1891 ) ;
#11097 = CARTESIAN_POINT ( 'NONE',  ( 10.00000000000000533, 5.421022142882375938, -1.761396867937200739 ) ) ;
#11098 =( NAMED_UNIT ( * ) SI_UNIT ( $, .STERADIAN. ) SOLID_ANGLE_UNIT ( ) );
#11099 = CYLINDRICAL_SURFACE ( 'NONE', #9756, 0.9999999999999974465 ) ;
#11100 = ORIENTED_EDGE ( 'NONE', *, *, #15282, .T. ) ;
#11101 = CARTESIAN_POINT ( 'NONE',  ( 5.668774803599156975, -0.5958122406256377568, -13.00000000000000533 ) ) ;
#11102 = AXIS2_PLACEMENT_3D ( 'NONE', #16941, #6309, #1729 ) ;
#11103 = CARTESIAN_POINT ( 'NONE',  ( -2.000000000000000444, 5.200000000000000178, 0.000000000000000000 ) ) ;
#11104 = CARTESIAN_POINT ( 'NONE',  ( 9.968749997951617203, 4.150607464521791634, 2.695436003842732298 ) ) ;
#11105 = CIRCLE ( 'NONE', #3114, 5.200000000000000178 ) ;
#11106 = CARTESIAN_POINT ( 'NONE',  ( -90.00000000000000000, 0.000000000000000000, 0.000000000000000000 ) ) ;
#11107 = CARTESIAN_POINT ( 'NONE',  ( -11.00000000000000355, 4.215373648918917304, -3.375000000000002665 ) ) ;
#11108 = ORIENTED_EDGE ( 'NONE', *, *, #8070, .T. ) ;
#11109 = DIRECTION ( 'NONE',  ( 1.000000000000000000, 0.000000000000000000, 0.000000000000000000 ) ) ;
#11110 = APPLICATION_CONTEXT ( 'automotive_design' ) ;
#11111 = DIRECTION ( 'NONE',  ( 0.000000000000000000, 0.000000000000000000, -1.000000000000000000 ) ) ;
#11112 = EDGE_CURVE ( 'NONE', #6062, #16380, #12309, .T. ) ;
#11113 = VERTEX_POINT ( 'NONE', #12205 ) ;
#11114 = DIRECTION ( 'NONE',  ( 0.000000000000000000, 1.000000000000000000, 0.000000000000000000 ) ) ;
#11115 = CARTESIAN_POINT ( 'NONE',  ( 10.58013454126452046, -14.56230589874905412, -32.00000000000000000 ) ) ;
#11116 = ORIENTED_EDGE ( 'NONE', *, *, #16931, .T. ) ;
#11117 = CIRCLE ( 'NONE', #5043, 1.000000000000002665 ) ;
#11118 = CIRCLE ( 'NONE', #15920, 0.9999999999999974465 ) ;
#11119 = CARTESIAN_POINT ( 'NONE',  ( 8.776855558857221240, 3.635492607468361559, 0.000000000000000000 ) ) ;
#11120 = CARTESIAN_POINT ( 'NONE',  ( 9.668198987696284163, -0.5990941410143687529, 5.700000000000001954 ) ) ;
#11121 = ORIENTED_EDGE ( 'NONE', *, *, #2266, .T. ) ;
#11122 = DIRECTION ( 'NONE',  ( 0.000000000000000000, 0.000000000000000000, 1.000000000000000000 ) ) ;
#11123 = DIRECTION ( 'NONE',  ( -1.000000000000000000, 0.000000000000000000, 0.000000000000000000 ) ) ;
#11124 = DIRECTION ( 'NONE',  ( 1.000000000000000000, 0.000000000000000000, 0.000000000000000000 ) ) ;
#11125 = EDGE_CURVE ( 'NONE', #2276, #10395, #12000, .T. ) ;
#11126 = EDGE_LOOP ( 'NONE', ( #711, #9780, #16025, #19435 ) ) ;
#11127 = ADVANCED_FACE ( 'NONE', ( #18693 ), #9303, .T. ) ;
#11128 = LINE ( 'NONE', #5018, #16944 ) ;
#11129 = ORIENTED_EDGE ( 'NONE', *, *, #11064, .T. ) ;
#11130 = ADVANCED_FACE ( 'NONE', ( #6470 ), #7219, .T. ) ;
#11131 = CARTESIAN_POINT ( 'NONE',  ( 1.493657965219485462, -5.574407415329169169, -14.81249999590322375 ) ) ;
#11132 = ORIENTED_EDGE ( 'NONE', *, *, #6233, .T. ) ;
#11133 = FACE_OUTER_BOUND ( 'NONE', #2331, .T. ) ;
#11134 = CARTESIAN_POINT ( 'NONE',  ( -4.780397808154247308, 1.280903732194486722, -14.34374999795161365 ) ) ;
#11135 = CYLINDRICAL_SURFACE ( 'NONE', #12002, 2.524999999999995914 ) ;
#11136 = AXIS2_PLACEMENT_3D ( 'NONE', #4363, #4066, #8768 ) ;
#11137 = CARTESIAN_POINT ( 'NONE',  ( 1.988169868018562880, -4.465502636338038123, -13.46874999795161543 ) ) ;
#11138 = EDGE_CURVE ( 'NONE', #13907, #8773, #16519, .T. ) ;
#11139 = ADVANCED_FACE ( 'NONE', ( #3396 ), #15994, .F. ) ;
#11140 = ORIENTED_EDGE ( 'NONE', *, *, #16536, .F. ) ;
#11141 = DIRECTION ( 'NONE',  ( 6.419766481290786633E-33, -1.000000000000000000, 0.000000000000000000 ) ) ;
#11142 = DIRECTION ( 'NONE',  ( 0.000000000000000000, 0.000000000000000000, -1.000000000000000000 ) ) ;
#11143 = ORIENTED_EDGE ( 'NONE', *, *, #162, .F. ) ;
#11144 =( BOUNDED_SURFACE ( )  B_SPLINE_SURFACE ( 1, 2, ( 
 ( #9820, #16115, #13200, #19007, #11406, #1093, #11598, #10106, #16208, #2482, #19390, #2577, #16299, #11314, #2391, #19099, #10203 ),
 ( #15912, #7168, #8595, #14412, #13291, #8505, #2193, #3797, #6073, #10694, #19486, #1487, #12189, #15299, #2981, #9095, #7472 ) ),
 .UNSPECIFIED., .F., .F., .F. ) 
 B_SPLINE_SURFACE_WITH_KNOTS ( ( 2, 2 ),
 ( 3, 2, 2, 2, 2, 2, 2, 2, 3 ),
 ( 0.000000000000000000, 1.000000000000000000 ),
 ( 0.000000000000000000, 0.05000000000000000278, 0.1000000000000000056, 0.1499999999999999944, 0.2000000000000000111, 0.2500000000000000000, 0.2999999999999999889, 0.3499999999999999778, 0.4000000000000000222 ),
 .UNSPECIFIED. ) 
 GEOMETRIC_REPRESENTATION_ITEM ( )  RATIONAL_B_SPLINE_SURFACE ( (
 ( 1.000000000000000000, 0.9876883405951377704, 1.000000000000000000, 0.9876883405951377704, 1.000000000000000000, 0.9876883405951377704, 1.000000000000000000, 0.9876883405951377704, 1.000000000000000000, 0.9876883405951377704, 1.000000000000000000, 0.9876883405951377704, 1.000000000000000000, 0.9876883405951377704, 1.000000000000000000, 0.9876883405951377704, 1.000000000000000000),
 ( 1.000000000000000000, 0.9876883405951377704, 1.000000000000000000, 0.9876883405951377704, 1.000000000000000000, 0.9876883405951377704, 1.000000000000000000, 0.9876883405951377704, 1.000000000000000000, 0.9876883405951377704, 1.000000000000000000, 0.9876883405951377704, 1.000000000000000000, 0.9876883405951377704, 1.000000000000000000, 0.9876883405951377704, 1.000000000000000000) ) ) 
 REPRESENTATION_ITEM ( '' )  SURFACE ( )  );
#11145 = DIRECTION ( 'NONE',  ( 0.000000000000000000, 0.000000000000000000, 1.000000000000000000 ) ) ;
#11146 = DIRECTION ( 'NONE',  ( 1.000000000000000000, 0.000000000000000000, 0.000000000000000000 ) ) ;
#11147 = CARTESIAN_POINT ( 'NONE',  ( 2.790000000000000036, 22.37986894186685660, -9.514945144208509120 ) ) ;
#11148 = AXIS2_PLACEMENT_3D ( 'NONE', #10354, #16451, #2095 ) ;
#11149 = EDGE_LOOP ( 'NONE', ( #8973, #11977, #1643, #13622 ) ) ;
#11150 = CARTESIAN_POINT ( 'NONE',  ( 11.00000000000000711, -2.849999999999954792, -4.936344801571327601 ) ) ;
#11151 = CARTESIAN_POINT ( 'NONE',  ( 6.843749997951615427, -4.233219804643852946, -2.444050593750049849 ) ) ;
#11152 = ORIENTED_EDGE ( 'NONE', *, *, #16598, .T. ) ;
#11153 = FACE_OUTER_BOUND ( 'NONE', #17818, .T. ) ;
#11154 = PRODUCT_RELATED_PRODUCT_CATEGORY ( 'part', '', ( #17368 ) ) ;
#11155 = ORIENTED_EDGE ( 'NONE', *, *, #12322, .T. ) ;
#11156 = APPLICATION_PROTOCOL_DEFINITION ( 'draft international standard', 'automotive_design', 1998, #2280 ) ;
#11157 = CARTESIAN_POINT ( 'NONE',  ( 6.560148031203755073E-16, 23.69843731927177544, -5.456805104200854295 ) ) ;
#11158 = COLOUR_RGB ( '', 0.09019608, 0.27058824, 0.51372549) ;
#11159 = CARTESIAN_POINT ( 'NONE',  ( 10.34374999795161543, 4.150607464521791634, 2.695436003842732298 ) ) ;
#11160 = ORIENTED_EDGE ( 'NONE', *, *, #13395, .F. ) ;
#11161 = ORIENTED_EDGE ( 'NONE', *, *, #11318, .F. ) ;
#11162 = CARTESIAN_POINT ( 'NONE',  ( -10.00000000000000000, 0.000000000000000000, 0.000000000000000000 ) ) ;
#11163 = CARTESIAN_POINT ( 'NONE',  ( 1.800000000000000488, 0.000000000000000000, -4.200000000000000178 ) ) ;
#11164 = ORIENTED_EDGE ( 'NONE', *, *, #9015, .F. ) ;
#11165 = ADVANCED_FACE ( 'NONE', ( #11588 ), #12699, .T. ) ;
#11166 = EDGE_CURVE ( 'NONE', #9602, #7536, #18994, .T. ) ;
#11167 = VECTOR ( 'NONE', #3537, 1000.000000000000000 ) ;
#11168 = FACE_OUTER_BOUND ( 'NONE', #911, .T. ) ;
#11169 = ORIENTED_EDGE ( 'NONE', *, *, #4174, .T. ) ;
#11170 = EDGE_CURVE ( 'NONE', #1219, #16193, #8188, .T. ) ;
#11171 = DIRECTION ( 'NONE',  ( 0.000000000000000000, 0.000000000000000000, 1.000000000000000000 ) ) ;
#11172 = LINE ( 'NONE', #359, #5511 ) ;
#11173 = DIRECTION ( 'NONE',  ( 1.000000000000000000, 0.000000000000000000, 0.000000000000000000 ) ) ;
#11174 = ORIENTED_EDGE ( 'NONE', *, *, #6619, .T. ) ;
#11175 = DIRECTION ( 'NONE',  ( 0.8191520442889917986, 1.003171929053524747E-16, -0.5735764363510460484 ) ) ;
#11176 = EDGE_CURVE ( 'NONE', #16982, #11206, #10436, .T. ) ;
#11177 = DIRECTION ( 'NONE',  ( -1.000000000000000000, 0.000000000000000000, 0.000000000000000000 ) ) ;
#11178 = EDGE_LOOP ( 'NONE', ( #13064, #17379 ) ) ;
#11179 = ORIENTED_EDGE ( 'NONE', *, *, #13484, .F. ) ;
#11180 = CARTESIAN_POINT ( 'NONE',  ( -3.814044456245444081, 4.235925505221192822, -12.00000000000000533 ) ) ;
#11181 = MECHANICAL_DESIGN_GEOMETRIC_PRESENTATION_REPRESENTATION (  '', ( #12465 ), #15665 ) ;
#11182 = DIRECTION ( 'NONE',  ( 0.000000000000000000, 0.000000000000000000, 1.000000000000000000 ) ) ;
#11183 = CARTESIAN_POINT ( 'NONE',  ( -5.142044285764750811, 2.620002426024544029, -7.500000000000005329 ) ) ;
#11184 = EDGE_LOOP ( 'NONE', ( #12386, #11883, #18663, #4823 ) ) ;
#11185 = CARTESIAN_POINT ( 'NONE',  ( 6.234374998975811266, -4.584782303107560963, -2.647025296875054057 ) ) ;
#11186 = CARTESIAN_POINT ( 'NONE',  ( 2.850000000000024070, 4.936344801571289409, -6.000000000000005329 ) ) ;
#11187 = VERTEX_POINT ( 'NONE', #888 ) ;
#11188 = FACE_OUTER_BOUND ( 'NONE', #7107, .T. ) ;
#11189 = EDGE_CURVE ( 'NONE', #4538, #6183, #1442, .T. ) ;
#11190 = DIRECTION ( 'NONE',  ( 1.000000000000000000, 0.000000000000000000, 0.000000000000000000 ) ) ;
#11191 = VECTOR ( 'NONE', #11402, 1000.000000000000000 ) ;
#11192 = AXIS2_PLACEMENT_3D ( 'NONE', #7616, #9133, #13633 ) ;
#11193 = DIRECTION ( 'NONE',  ( -1.000000000000000000, 0.000000000000000000, 0.000000000000000000 ) ) ;
#11194 = CARTESIAN_POINT ( 'NONE',  ( 0.02436607992775891365, -24.63872515616080960, -2.336989772644527008 ) ) ;
#11195 = CARTESIAN_POINT ( 'NONE',  ( -3.954556930911881096, -2.873153789725797935, -14.46874999795161720 ) ) ;
#11196 = DIRECTION ( 'NONE',  ( 0.000000000000000000, 0.000000000000000000, -1.000000000000000000 ) ) ;
#11197 = FACE_OUTER_BOUND ( 'NONE', #7620, .T. ) ;
#11198 = CARTESIAN_POINT ( 'NONE',  ( -1.185096637661215535, 5.575441324182696334, -8.312499995903225525 ) ) ;
#11199 = ORIENTED_EDGE ( 'NONE', *, *, #15781, .F. ) ;
#11200 = CARTESIAN_POINT ( 'NONE',  ( 2.789999999999999147, -23.48180575137726223, -5.535312321042966666 ) ) ;
#11201 = FILL_AREA_STYLE_COLOUR ( '', #4900 ) ;
#11202 = UNCERTAINTY_MEASURE_WITH_UNIT (LENGTH_MEASURE( 1.000000000000000082E-05 ), #11473, 'distance_accuracy_value', 'NONE');
#11203 = LINE ( 'NONE', #14303, #14394 ) ;
#11204 = FACE_OUTER_BOUND ( 'NONE', #1201, .T. ) ;
#11205 = CARTESIAN_POINT ( 'NONE',  ( 0.000000000000000000, 0.000000000000000000, -29.00000000000000000 ) ) ;
#11206 = VERTEX_POINT ( 'NONE', #17691 ) ;
#11207 = CARTESIAN_POINT ( 'NONE',  ( 0.02436607992776585255, -5.391175441198789109, 24.15498966839961170 ) ) ;
#11208 = TOROIDAL_SURFACE ( 'NONE', #17603, 24.12539914357697768, 8.000000000000000000 ) ;
#11209 = DIRECTION ( 'NONE',  ( -4.163336342344335449E-15, 1.000000000000000000, 0.000000000000000000 ) ) ;
#11210 = AXIS2_PLACEMENT_3D ( 'NONE', #599, #1991, #6776 ) ;
#11211 = ORIENTED_EDGE ( 'NONE', *, *, #774, .F. ) ;
#11212 = LINE ( 'NONE', #3701, #11876 ) ;
#11213 = CARTESIAN_POINT ( 'NONE',  ( 0.02436607992775674525, 9.836394144776026138, -22.71065055754441531 ) ) ;
#11214 = ORIENTED_EDGE ( 'NONE', *, *, #6593, .T. ) ;
#11215 = DIRECTION ( 'NONE',  ( 0.000000000000000000, -1.000000000000000000, 0.000000000000000000 ) ) ;
#11216 = CARTESIAN_POINT ( 'NONE',  ( 12.50000000000000533, -4.840010801796506001, 3.143139765844590983 ) ) ;
#11217 = B_SPLINE_CURVE_WITH_KNOTS ( 'NONE', 3,
 ( #3084, #6364, #13996, #15304 ),
 .UNSPECIFIED., .F., .F.,
 ( 4, 4 ),
 ( 2.135345996173299606E-07, 0.0006888010880210790939 ),
 .UNSPECIFIED. ) ;
#11218 = ORIENTED_EDGE ( 'NONE', *, *, #19377, .F. ) ;
#11219 = VECTOR ( 'NONE', #11702, 1000.000000000000000 ) ;
#11220 = FACE_OUTER_BOUND ( 'NONE', #12878, .T. ) ;
#11221 = CARTESIAN_POINT ( 'NONE',  ( -3.814044456245444081, 4.235925505221192822, -13.31249999590322730 ) ) ;
#11222 = DIRECTION ( 'NONE',  ( 1.000000000000000000, 0.000000000000000000, 0.000000000000000000 ) ) ;
#11223 = EDGE_CURVE ( 'NONE', #18420, #14758, #18736, .T. ) ;
#11224 = ORIENTED_EDGE ( 'NONE', *, *, #15296, .F. ) ;
#11225 = CARTESIAN_POINT ( 'NONE',  ( 5.700000000000001954, 0.000000000000000000, 0.000000000000000000 ) ) ;
#11226 = ORIENTED_EDGE ( 'NONE', *, *, #14377, .T. ) ;
#11227 = LINE ( 'NONE', #8121, #3762 ) ;
#11228 = ORIENTED_EDGE ( 'NONE', *, *, #1400, .T. ) ;
#11229 = CARTESIAN_POINT ( 'NONE',  ( 2.499999999999998668, 8.800000000000023803, 0.000000000000000000 ) ) ;
#11230 = CARTESIAN_POINT ( 'NONE',  ( 9.000000000000000000, 1.102182119232617714E-15, -29.00000000000000000 ) ) ;
#11231 = CARTESIAN_POINT ( 'NONE',  ( 2.789999999999999147, -20.70663861606260170, -15.04425356660783031 ) ) ;
#11232 = CARTESIAN_POINT ( 'NONE',  ( 0.02436607992776064838, 18.55949924794892780, 16.37294372382865504 ) ) ;
#11233 = ORIENTED_EDGE ( 'NONE', *, *, #15175, .T. ) ;
#11234 = DIRECTION ( 'NONE',  ( -1.000000000000000000, -0.000000000000000000, -0.000000000000000000 ) ) ;
#11235 = DIRECTION ( 'NONE',  ( -1.000000000000000000, -0.000000000000000000, 0.000000000000000000 ) ) ;
#11236 = AXIS2_PLACEMENT_3D ( 'NONE', #14142, #9857, #18841 ) ;
#11237 = ORIENTED_EDGE ( 'NONE', *, *, #12373, .F. ) ;
#11238 = AXIS2_PLACEMENT_3D ( 'NONE', #14081, #12193, #2983 ) ;
#11239 = EDGE_CURVE ( 'NONE', #16572, #11644, #6900, .T. ) ;
#11240 = CYLINDRICAL_SURFACE ( 'NONE', #19254, 1.000000000000000000 ) ;
#11241 = CARTESIAN_POINT ( 'NONE',  ( 50.00050000000000239, 0.000000000000000000, 0.000000000000000000 ) ) ;
#11242 = CARTESIAN_POINT ( 'NONE',  ( 2.444050593749960587, -4.233219804643904460, -6.468749997951615427 ) ) ;
#11243 = ORIENTED_EDGE ( 'NONE', *, *, #11379, .T. ) ;
#11244 = CARTESIAN_POINT ( 'NONE',  ( -15.00000000000000355, 1.224646799147353454E-16, 0.000000000000000000 ) ) ;
#11245 = CARTESIAN_POINT ( 'NONE',  ( -11.00000000000000355, 4.898587196589412829E-16, 0.000000000000000000 ) ) ;
#11246 = CARTESIAN_POINT ( 'NONE',  ( 10.84374999795161543, -1.016293382781444654, 4.781284448697187273 ) ) ;
#11247 = EDGE_CURVE ( 'NONE', #12336, #6290, #1805, .T. ) ;
#11248 = EDGE_LOOP ( 'NONE', ( #1024, #11088, #17982, #15008 ) ) ;
#11249 = PLANE ( 'NONE',  #15476 ) ;
#11250 = VECTOR ( 'NONE', #5809, 1000.000000000000000 ) ;
#11251 = ORIENTED_EDGE ( 'NONE', *, *, #2136, .T. ) ;
#11252 = AXIS2_PLACEMENT_3D ( 'NONE', #1661, #7759, #16975 ) ;
#11253 = CARTESIAN_POINT ( 'NONE',  ( 10.84374999795161543, -1.016293382781444654, 4.781284448697187273 ) ) ;
#11254 = CARTESIAN_POINT ( 'NONE',  ( 2.789999999999999147, 14.55412442567617681, 19.64056340710880022 ) ) ;
#11255 = ORIENTED_EDGE ( 'NONE', *, *, #17661, .F. ) ;
#11256 = EDGE_LOOP ( 'NONE', ( #12849, #4411, #17182, #14228, #16930, #3841 ) ) ;
#11257 = DIRECTION ( 'NONE',  ( 0.000000000000000000, 0.000000000000000000, -1.000000000000000000 ) ) ;
#11258 = DIRECTION ( 'NONE',  ( 0.000000000000000000, 0.000000000000000000, -1.000000000000000000 ) ) ;
#11259 = CYLINDRICAL_SURFACE ( 'NONE', #8554, 0.9999999999999974465 ) ;
#11260 = ORIENTED_EDGE ( 'NONE', *, *, #8076, .T. ) ;
#11261 = MECHANICAL_DESIGN_GEOMETRIC_PRESENTATION_REPRESENTATION (  '', ( #18280 ), #12214 ) ;
#11262 = PRESENTATION_STYLE_ASSIGNMENT (( #6840 ) ) ;
#11263 = ADVANCED_FACE ( 'NONE', ( #6671 ), #6571, .F. ) ;
#11264 = CIRCLE ( 'NONE', #5805, 4.400000000000000355 ) ;
#11265 = ORIENTED_EDGE ( 'NONE', *, *, #16897, .F. ) ;
#11266 = AXIS2_PLACEMENT_3D ( 'NONE', #1369, #969, #11576 ) ;
#11267 = VECTOR ( 'NONE', #4480, 1000.000000000000000 ) ;
#11268 = EDGE_CURVE ( 'NONE', #12799, #3536, #12369, .T. ) ;
#11269 = CARTESIAN_POINT ( 'NONE',  ( -1.493657965219562511, -5.574407415329147852, -8.500000000000005329 ) ) ;
#11270 = VECTOR ( 'NONE', #16666, 1000.000000000000000 ) ;
#11271 = DIRECTION ( 'NONE',  ( -1.000000000000000000, 0.000000000000000000, 0.000000000000000000 ) ) ;
#11272 = CARTESIAN_POINT ( 'NONE',  ( 4.476417968967386862, 17.43449690031536292, -32.00000000000000000 ) ) ;
#11273 = EDGE_CURVE ( 'NONE', #8799, #676, #19087, .T. ) ;
#11274 = ORIENTED_EDGE ( 'NONE', *, *, #7324, .F. ) ;
#11275 = CARTESIAN_POINT ( 'NONE',  ( 5.139549990269394683E-16, -2.133490293297187979, 24.22479935914660132 ) ) ;
#11276 =( NAMED_UNIT ( * ) PLANE_ANGLE_UNIT ( ) SI_UNIT ( $, .RADIAN. ) );
#11277 = DIRECTION ( 'NONE',  ( 0.000000000000000000, 0.000000000000000000, 1.000000000000000000 ) ) ;
#11278 = VERTEX_POINT ( 'NONE', #8085 ) ;
#11279 = VERTEX_POINT ( 'NONE', #14296 ) ;
#11280 = DIRECTION ( 'NONE',  ( 1.000000000000000000, 0.000000000000000000, 0.000000000000000000 ) ) ;
#11281 = CIRCLE ( 'NONE', #16707, 2.524999999999998135 ) ;
#11282 = EDGE_CURVE ( 'NONE', #4912, #6438, #17784, .T. ) ;
#11283 = DIRECTION ( 'NONE',  ( -1.000000000000000000, 0.000000000000000000, 0.000000000000000000 ) ) ;
#11284 = CIRCLE ( 'NONE', #18308, 2.524999999999995914 ) ;
#11285 = PLANE ( 'NONE',  #8498 ) ;
#11286 = ORIENTED_EDGE ( 'NONE', *, *, #16462, .F. ) ;
#11287 = DIRECTION ( 'NONE',  ( 0.000000000000000000, 0.000000000000000000, 1.000000000000000000 ) ) ;
#11288 = PRESENTATION_LAYER_ASSIGNMENT (  '', '', ( #6157 ) ) ;
#11289 = CARTESIAN_POINT ( 'NONE',  ( -2.000000000000000000, -8.000000000000003553, 37.99999999999999289 ) ) ;
#11290 = ORIENTED_EDGE ( 'NONE', *, *, #13059, .F. ) ;
#11291 = CARTESIAN_POINT ( 'NONE',  ( 8.000000000000000000, 0.000000000000000000, 0.000000000000000000 ) ) ;
#11292 = ADVANCED_FACE ( 'NONE', ( #3785 ), #597, .F. ) ;
#11293 = EDGE_CURVE ( 'NONE', #307, #13120, #12032, .T. ) ;
#11294 = DIRECTION ( 'NONE',  ( 1.000000000000000000, -0.000000000000000000, -0.000000000000000000 ) ) ;
#11295 =( GEOMETRIC_REPRESENTATION_CONTEXT ( 3 ) GLOBAL_UNCERTAINTY_ASSIGNED_CONTEXT ( ( #16396 ) ) GLOBAL_UNIT_ASSIGNED_CONTEXT ( ( #14717, #7182, #5594 ) ) REPRESENTATION_CONTEXT ( 'NONE', 'WORKASPACE' ) );
#11296 = DIRECTION ( 'NONE',  ( -1.000000000000000000, -0.000000000000000000, -0.000000000000000000 ) ) ;
#11297 = DIRECTION ( 'NONE',  ( 0.000000000000000000, 1.000000000000000000, -1.224646799147353207E-16 ) ) ;
#11298 = CARTESIAN_POINT ( 'NONE',  ( 2.999999999999998224, -2.487173708821168283, 2.318181818181817455 ) ) ;
#11299 = ADVANCED_FACE ( 'NONE', ( #9907 ), #18191, .T. ) ;
#11300 = CARTESIAN_POINT ( 'NONE',  ( 10.31249999590322552, 0.5958122406255991210, 5.668774803599163192 ) ) ;
#11301 = DIRECTION ( 'NONE',  ( -0.000000000000000000, -0.000000000000000000, 1.000000000000000000 ) ) ;
#11302 = CIRCLE ( 'NONE', #13536, 0.9999999999999974465 ) ;
#11303 = SURFACE_SIDE_STYLE ('',( #17595 ) ) ;
#11304 = VERTEX_POINT ( 'NONE', #5962 ) ;
#11305 = LINE ( 'NONE', #17405, #9866 ) ;
#11306 = DIRECTION ( 'NONE',  ( -4.163336342344335449E-15, 1.000000000000000000, 0.000000000000000000 ) ) ;
#11307 = CARTESIAN_POINT ( 'NONE',  ( -36.00000000000000000, -5.000000000000001776, 5.000000000000000000 ) ) ;
#11308 = EDGE_CURVE ( 'NONE', #3152, #13990, #8981, .T. ) ;
#11309 = CARTESIAN_POINT ( 'NONE',  ( 7.000000000000005329, 3.814044456245473835, 4.235925505221166176 ) ) ;
#11310 = DIRECTION ( 'NONE',  ( -0.000000000000000000, -0.000000000000000000, -1.000000000000000000 ) ) ;
#11311 = VERTEX_POINT ( 'NONE', #11881 ) ;
#11312 = CARTESIAN_POINT ( 'NONE',  ( 2.789999999999999147, 20.70663861606293210, -15.04425356660737556 ) ) ;
#11313 =( GEOMETRIC_REPRESENTATION_CONTEXT ( 3 ) GLOBAL_UNCERTAINTY_ASSIGNED_CONTEXT ( ( #13004 ) ) GLOBAL_UNIT_ASSIGNED_CONTEXT ( ( #294, #3589, #11098 ) ) REPRESENTATION_CONTEXT ( 'NONE', 'WORKASPACE' ) );
#11314 = CARTESIAN_POINT ( 'NONE',  ( 2.620002426024544029, 5.142044285764750811, -13.81249999590322552 ) ) ;
#11315 = ORIENTED_EDGE ( 'NONE', *, *, #423, .T. ) ;
#11316 = CARTESIAN_POINT ( 'NONE',  ( 7.843749997951614539, -1.510506337161893864, 4.648860486681943627 ) ) ;
#11317 = CARTESIAN_POINT ( 'NONE',  ( 0.02436607992776368414, -9.836394144775550075, -22.71065055754462492 ) ) ;
#11318 = EDGE_CURVE ( 'NONE', #1730, #750, #8522, .T. ) ;
#11319 = EDGE_LOOP ( 'NONE', ( #5196, #19458, #14967, #16942 ) ) ;
#11320 = CARTESIAN_POINT ( 'NONE',  ( -4.200000000000000178, 5.143516556418885886E-16, -28.99999999999999645 ) ) ;
#11321 = TOROIDAL_SURFACE ( 'NONE', #2670, 6.760799999999997034, 0.03079999999999868954 ) ;
#11322 = B_SPLINE_CURVE_WITH_KNOTS ( 'NONE', 3,
 ( #3739, #5334, #9760, #14347, #6720, #12846 ),
 .UNSPECIFIED., .F., .F.,
 ( 4, 2, 4 ),
 ( 2.032124546189838441E-07, 0.001878594002992310316, 0.003756984793530001362 ),
 .UNSPECIFIED. ) ;
#11323 = CARTESIAN_POINT ( 'NONE',  ( 0.07181525696555157712, 5.344212458769712626, -24.78695292654915860 ) ) ;
#11324 = CARTESIAN_POINT ( 'NONE',  ( 3.968750000000000000, 0.000000000000000000, -5.946610266546040968 ) ) ;
#11325 = CARTESIAN_POINT ( 'NONE',  ( 13.00000000000000000, 5.567819778318904511, 1.220402768007685657 ) ) ;
#11326 = ORIENTED_EDGE ( 'NONE', *, *, #2785, .T. ) ;
#11327 = STYLED_ITEM ( 'NONE', ( #18672 ), #3271 ) ;
#11328 = AXIS2_PLACEMENT_3D ( 'NONE', #12560, #7745, #17353 ) ;
#11329 = CARTESIAN_POINT ( 'NONE',  ( -5.209999999999999964, 0.000000000000000000, 0.000000000000000000 ) ) ;
#11330 = CARTESIAN_POINT ( 'NONE',  ( 0.2436698586202201144, 7.118259520043989361E-16, -4.824999999999999289 ) ) ;
#11331 = FACE_OUTER_BOUND ( 'NONE', #12748, .T. ) ;
#11332 = ORIENTED_EDGE ( 'NONE', *, *, #542, .F. ) ;
#11333 = CARTESIAN_POINT ( 'NONE',  ( 11.46874999795161543, -4.888101187500000222, -3.383411828340740850E-14 ) ) ;
#11334 = EDGE_LOOP ( 'NONE', ( #3010, #19309, #12459, #13884 ) ) ;
#11335 = DIRECTION ( 'NONE',  ( -1.000000000000000000, -6.419766481290786633E-33, 0.000000000000000000 ) ) ;
#11336 = VERTEX_POINT ( 'NONE', #8680 ) ;
#11337 = CARTESIAN_POINT ( 'NONE',  ( -2.000000000000001776, 6.500000000000000000, 0.000000000000000000 ) ) ;
#11338 = CARTESIAN_POINT ( 'NONE',  ( 1.039999999999997149, -4.633866840648735774, -27.68468304288263226 ) ) ;
#11339 = DIRECTION ( 'NONE',  ( 0.000000000000000000, 0.000000000000000000, 1.000000000000000000 ) ) ;
#11340 = CARTESIAN_POINT ( 'NONE',  ( 2.695436003842704764, -4.150607464521812062, -13.34374999795161365 ) ) ;
#11341 = ORIENTED_EDGE ( 'NONE', *, *, #1859, .F. ) ;
#11342 = CARTESIAN_POINT ( 'NONE',  ( 2.765633920072237295, 12.59161484032912171, 21.30679549418635688 ) ) ;
#11343 = DIRECTION ( 'NONE',  ( 0.000000000000000000, 0.000000000000000000, 1.000000000000000000 ) ) ;
#11344 = EDGE_LOOP ( 'NONE', ( #14909, #18337, #1902, #15481 ) ) ;
#11345 = B_SPLINE_CURVE_WITH_KNOTS ( 'NONE', 3,
 ( #13535, #2724, #19639, #5922, #18144, #7516 ),
 .UNSPECIFIED., .F., .F.,
 ( 4, 2, 4 ),
 ( 4.462636882273700183E-07, 0.001879885203074810199, 0.003759324142461393028 ),
 .UNSPECIFIED. ) ;
#11346 = ADVANCED_FACE ( 'NONE', ( #7356 ), #7545, .T. ) ;
#11347 = DIRECTION ( 'NONE',  ( -1.000000000000000000, -6.419766481290786633E-33, 0.000000000000000000 ) ) ;
#11348 = AXIS2_PLACEMENT_3D ( 'NONE', #12408, #3296, #2087 ) ;
#11349 = DIRECTION ( 'NONE',  ( 0.000000000000000000, 0.000000000000000000, 1.000000000000000000 ) ) ;
#11350 = DIRECTION ( 'NONE',  ( 0.000000000000000000, 0.000000000000000000, -1.000000000000000000 ) ) ;
#11351 = EDGE_LOOP ( 'NONE', ( #18212, #13072, #7543, #18216 ) ) ;
#11352 = DIRECTION ( 'NONE',  ( 0.000000000000000000, 0.000000000000000000, -1.000000000000000000 ) ) ;
#11353 = EDGE_CURVE ( 'NONE', #758, #16305, #15565, .T. ) ;
#11354 = CARTESIAN_POINT ( 'NONE',  ( 5.142044285764733935, -2.620002426024580000, -7.500000000000005329 ) ) ;
#11355 = CARTESIAN_POINT ( 'NONE',  ( -1.869200000000000195, 0.000000000000000000, 0.000000000000000000 ) ) ;
#11356 = VERTEX_POINT ( 'NONE', #4180 ) ;
#11357 = DIRECTION ( 'NONE',  ( 0.000000000000000000, 0.000000000000000000, 1.000000000000000000 ) ) ;
#11358 = CIRCLE ( 'NONE', #5589, 5.700000000000001954 ) ;
#11359 = ORIENTED_EDGE ( 'NONE', *, *, #18835, .F. ) ;
#11360 = ITEM_DEFINED_TRANSFORMATION ( 'NONE', 'NONE', #13066,  #16724 ) ;
#11361 = PRESENTATION_STYLE_ASSIGNMENT (( #3942 ) ) ;
#11362 = ORIENTED_EDGE ( 'NONE', *, *, #14312, .T. ) ;
#11363 = VERTEX_POINT ( 'NONE', #16389 ) ;
#11364 = CARTESIAN_POINT ( 'NONE',  ( 0.06562551705663710599, -21.84204283372370625, 12.72258903105631234 ) ) ;
#11365 = CARTESIAN_POINT ( 'NONE',  ( 12.31249999590322552, -5.700000000000001066, -3.945386292505473391E-14 ) ) ;
#11366 = CARTESIAN_POINT ( 'NONE',  ( 11.96874999795161365, -3.114526743279282250, 3.846120219227923798 ) ) ;
#11367 = VERTEX_POINT ( 'NONE', #13580 ) ;
#11368 = EDGE_CURVE ( 'NONE', #17179, #9124, #19681, .T. ) ;
#11369 = CARTESIAN_POINT ( 'NONE',  ( -1.988169868018530906, 4.465502636338051445, -13.84374999795161543 ) ) ;
#11370 = ORIENTED_EDGE ( 'NONE', *, *, #17394, .T. ) ;
#11371 = CIRCLE ( 'NONE', #19033, 1.000000000000003109 ) ;
#11372 = CARTESIAN_POINT ( 'NONE',  ( -10.00000000000000000, 0.000000000000000000, 0.000000000000000000 ) ) ;
#11373 = CARTESIAN_POINT ( 'NONE',  ( 9.000000000000005329, -4.611396867937225252, 3.350375938067065462 ) ) ;
#11374 = DIRECTION ( 'NONE',  ( 0.000000000000000000, 6.870191984066572599E-15, -1.000000000000000000 ) ) ;
#11375 = VERTEX_POINT ( 'NONE', #16589 ) ;
#11376 = CARTESIAN_POINT ( 'NONE',  ( 0.000000000000000000, 0.000000000000000000, 0.000000000000000000 ) ) ;
#11377 = ORIENTED_EDGE ( 'NONE', *, *, #16487, .F. ) ;
#11378 = EDGE_CURVE ( 'NONE', #19481, #10551, #5637, .T. ) ;
#11379 = EDGE_CURVE ( 'NONE', #1540, #7513, #10465, .T. ) ;
#11380 = ORIENTED_EDGE ( 'NONE', *, *, #1920, .F. ) ;
#11381 = CARTESIAN_POINT ( 'NONE',  ( -8.671566133830875600, 15.77352024078954429, 32.00000000000000000 ) ) ;
#11382 = AXIS2_PLACEMENT_3D ( 'NONE', #8824, #2706, #5803 ) ;
#11383 = CARTESIAN_POINT ( 'NONE',  ( -2.000000000000001776, 0.000000000000000000, 0.000000000000000000 ) ) ;
#11384 = CARTESIAN_POINT ( 'NONE',  ( 2.563317066925346527E-16, -12.51294990530000817, -20.85230829256867935 ) ) ;
#11385 = VERTEX_POINT ( 'NONE', #4379 ) ;
#11386 = CARTESIAN_POINT ( 'NONE',  ( 8.968749997951611874, -1.280903732194386579, -4.780397808154273953 ) ) ;
#11387 = CARTESIAN_POINT ( 'NONE',  ( 13.00000000000000178, -3.789407127742538517, 3.087705756618167374 ) ) ;
#11388 = ORIENTED_EDGE ( 'NONE', *, *, #13649, .F. ) ;
#11389 = CARTESIAN_POINT ( 'NONE',  ( 1.394999999999999574, 12.52377138324259676, -25.12109765559640451 ) ) ;
#11390 = CARTESIAN_POINT ( 'NONE',  ( 12.50000000000000533, 5.142044285764751699, 2.620002426024544029 ) ) ;
#11391 = AXIS2_PLACEMENT_3D ( 'NONE', #620, #6696, #18917 ) ;
#11392 = AXIS2_PLACEMENT_3D ( 'NONE', #4098, #19293, #5585 ) ;
#11393 = DIRECTION ( 'NONE',  ( 1.000000000000000000, 0.000000000000000000, -0.000000000000000000 ) ) ;
#11394 = CARTESIAN_POINT ( 'NONE',  ( 91.50000000000000000, 0.000000000000000000, 4.000000000000000000 ) ) ;
#11395 = CARTESIAN_POINT ( 'NONE',  ( -0.7741991708319226895, -4.888101187499994893, -11.96874999795161365 ) ) ;
#11396 = DIRECTION ( 'NONE',  ( 0.000000000000000000, 0.000000000000000000, 1.000000000000000000 ) ) ;
#11397 = CARTESIAN_POINT ( 'NONE',  ( 2.780897501012522977, 21.10878525316979903, -12.54316204260869760 ) ) ;
#11398 = ORIENTED_EDGE ( 'NONE', *, *, #12307, .T. ) ;
#11399 = FACE_OUTER_BOUND ( 'NONE', #2945, .T. ) ;
#11400 = DIRECTION ( 'NONE',  ( 1.000000000000000000, 0.000000000000000000, 0.000000000000000000 ) ) ;
#11401 = UNCERTAINTY_MEASURE_WITH_UNIT (LENGTH_MEASURE( 1.000000000000000082E-05 ), #9686, 'distance_accuracy_value', 'NONE');
#11402 = DIRECTION ( 'NONE',  ( -1.000000000000000000, 0.000000000000000000, 0.000000000000000000 ) ) ;
#11403 = CARTESIAN_POINT ( 'NONE',  ( 14.84374999795161543, 1.988169868018623720, -4.465502636338010589 ) ) ;
#11404 = CARTESIAN_POINT ( 'NONE',  ( 11.32184790671639263, 13.12143529358541016, 35.00000000000000000 ) ) ;
#11405 = VECTOR ( 'NONE', #14910, 1000.000000000000000 ) ;
#11406 = CARTESIAN_POINT ( 'NONE',  ( -4.611396867937201272, 3.350375938067097437, -9.312499995903225525 ) ) ;
#11407 = VECTOR ( 'NONE', #12831, 1000.000000000000000 ) ;
#11408 = ORIENTED_EDGE ( 'NONE', *, *, #16681, .F. ) ;
#11409 = EDGE_CURVE ( 'NONE', #15039, #15498, #16491, .T. ) ;
#11410 = CARTESIAN_POINT ( 'NONE',  ( 12.31249999590322552, -5.700000000000001066, -3.945386292505473391E-14 ) ) ;
#11411 = CIRCLE ( 'NONE', #7877, 6.543750000000017941 ) ;
#11412 = ADVANCED_FACE ( 'NONE', ( #19478 ), #16532, .T. ) ;
#11413 = CARTESIAN_POINT ( 'NONE',  ( 0.07181525068722525995, 25.22524549359950541, -2.576941577947494011 ) ) ;
#11414 = ORIENTED_EDGE ( 'NONE', *, *, #2767, .T. ) ;
#11415 = DIRECTION ( 'NONE',  ( 0.000000000000000000, 0.000000000000000000, -1.000000000000000000 ) ) ;
#11416 = CARTESIAN_POINT ( 'NONE',  ( 1.039999999999995595, 4.147968289691676524, -27.76164181293047051 ) ) ;
#11417 = EDGE_CURVE ( 'NONE', #12785, #2600, #2472, .T. ) ;
#11418 = CARTESIAN_POINT ( 'NONE',  ( -15.00000000000000355, 1.224646799147353454E-16, 0.000000000000000000 ) ) ;
#11419 = CARTESIAN_POINT ( 'NONE',  ( 2.789999999999999147, -5.391175441198789109, 24.15498966839961170 ) ) ;
#11420 = EDGE_LOOP ( 'NONE', ( #17469, #6686, #6613, #13042 ) ) ;
#11421 = VECTOR ( 'NONE', #13978, 1000.000000000000000 ) ;
#11422 = CARTESIAN_POINT ( 'NONE',  ( -2.000000000000000000, 1.999999999999998224, 37.99999999999999289 ) ) ;
#11423 = SURFACE_SIDE_STYLE ('',( #19499 ) ) ;
#11424 = CARTESIAN_POINT ( 'NONE',  ( 2.257825477245765988, -19.66801664102690239, -18.57583492944443293 ) ) ;
#11425 = VECTOR ( 'NONE', #2653, 1000.000000000000000 ) ;
#11426 = ORIENTED_EDGE ( 'NONE', *, *, #7008, .T. ) ;
#11427 = CARTESIAN_POINT ( 'NONE',  ( 12.96874999795161543, -4.409619785863891472, -2.246813503491864150 ) ) ;
#11428 = ORIENTED_EDGE ( 'NONE', *, *, #13519, .F. ) ;
#11429 = DIRECTION ( 'NONE',  ( 0.000000000000000000, 0.000000000000000000, 1.000000000000000000 ) ) ;
#11430 = VERTEX_POINT ( 'NONE', #8583 ) ;
#11431 = ADVANCED_FACE ( 'NONE', ( #980 ), #17887, .F. ) ;
#11432 = CARTESIAN_POINT ( 'NONE',  ( 1.039999999999997593, -12.52377138324241557, 25.12109765559648977 ) ) ;
#11433 = PLANE ( 'NONE',  #6917 ) ;
#11434 = FACE_OUTER_BOUND ( 'NONE', #2510, .T. ) ;
#11435 = DIRECTION ( 'NONE',  ( 0.000000000000000000, 0.000000000000000000, 1.000000000000000000 ) ) ;
#11436 = ORIENTED_EDGE ( 'NONE', *, *, #2441, .F. ) ;
#11437 = CARTESIAN_POINT ( 'NONE',  ( 1.773574444220693103, -4.620319390059841602, -7.343749997951615427 ) ) ;
#11438 = SHAPE_REPRESENTATION ( 'double end studs bm=1.5d_am_AM A M8X100-N', ( #16724 ), #16405 ) ;
#11439 = CARTESIAN_POINT ( 'NONE',  ( -0.2436698586202288019, 8.786840783882257924E-16, -7.174999999999998934 ) ) ;
#11440 = CIRCLE ( 'NONE', #11747, 1.000000000000002665 ) ;
#11441 = ORIENTED_EDGE ( 'NONE', *, *, #286, .T. ) ;
#11442 = DIRECTION ( 'NONE',  ( 1.000000000000000000, 0.000000000000000000, 0.000000000000000000 ) ) ;
#11443 = EDGE_CURVE ( 'NONE', #10821, #8477, #13192, .T. ) ;
#11444 = FACE_OUTER_BOUND ( 'NONE', #4046, .T. ) ;
#11445 = CARTESIAN_POINT ( 'NONE',  ( 4.888101187499994893, -0.7741991708319229115, -7.343749997951615427 ) ) ;
#11446 = ORIENTED_EDGE ( 'NONE', *, *, #6637, .T. ) ;
#11447 = DIRECTION ( 'NONE',  ( 0.000000000000000000, 0.000000000000000000, -1.000000000000000000 ) ) ;
#11448 = CARTESIAN_POINT ( 'NONE',  ( 3.350375938067065462, -4.611396867937225252, -9.000000000000005329 ) ) ;
#11449 = CARTESIAN_POINT ( 'NONE',  ( 2.000000000000000000, 1.999999999999997335, 37.99999999999999289 ) ) ;
#11450 = ORIENTED_EDGE ( 'NONE', *, *, #3360, .T. ) ;
#11451 = CARTESIAN_POINT ( 'NONE',  ( -15.00000000000000355, 1.224646799147353454E-16, 0.000000000000000000 ) ) ;
#11452 = CIRCLE ( 'NONE', #7921, 8.000000000000000000 ) ;
#11453 = EDGE_CURVE ( 'NONE', #8180, #9399, #13283, .T. ) ;
#11454 = VERTEX_POINT ( 'NONE', #11785 ) ;
#11455 = DIRECTION ( 'NONE',  ( 0.000000000000000000, 0.000000000000000000, 1.000000000000000000 ) ) ;
#11456 = AXIS2_PLACEMENT_3D ( 'NONE', #2294, #5581, #6977 ) ;
#11457 = DIRECTION ( 'NONE',  ( 0.000000000000000000, 0.000000000000000000, 1.000000000000000000 ) ) ;
#11458 = DIRECTION ( 'NONE',  ( -1.000000000000000000, -0.000000000000000000, 0.000000000000000000 ) ) ;
#11459 = VERTEX_POINT ( 'NONE', #19380 ) ;
#11460 = EDGE_LOOP ( 'NONE', ( #7746, #5880, #9096, #9085 ) ) ;
#11461 = CARTESIAN_POINT ( 'NONE',  ( -5.700000000000001066, 0.000000000000000000, -6.000000000000005329 ) ) ;
#11462 = DIRECTION ( 'NONE',  ( 0.000000000000000000, 0.000000000000000000, 1.000000000000000000 ) ) ;
#11463 = DIRECTION ( 'NONE',  ( 1.000000000000000000, 0.000000000000000000, 0.000000000000000000 ) ) ;
#11464 = ORIENTED_EDGE ( 'NONE', *, *, #11417, .F. ) ;
#11465 = PRODUCT_DEFINITION_SHAPE ( 'NONE', 'NONE',  #396 ) ;
#11466 = ORIENTED_EDGE ( 'NONE', *, *, #14853, .F. ) ;
#11467 = EDGE_CURVE ( 'NONE', #19481, #9137, #10292, .T. ) ;
#11468 = CARTESIAN_POINT ( 'NONE',  ( 0.000000000000000000, 0.000000000000000000, 0.000000000000000000 ) ) ;
#11469 = STYLED_ITEM ( 'NONE', ( #19259 ), #1118 ) ;
#11470 = CARTESIAN_POINT ( 'NONE',  ( 91.50000000000000000, 0.000000000000000000, 0.000000000000000000 ) ) ;
#11471 = ORIENTED_EDGE ( 'NONE', *, *, #12016, .F. ) ;
#11472 = CARTESIAN_POINT ( 'NONE',  ( -4.781284448697179279, 1.016293382781477961, -10.84374999795161543 ) ) ;
#11473 =( LENGTH_UNIT ( ) NAMED_UNIT ( * ) SI_UNIT ( .MILLI., .METRE. ) );
#11474 = EDGE_CURVE ( 'NONE', #16477, #14603, #309, .T. ) ;
#11475 = ORIENTED_EDGE ( 'NONE', *, *, #11653, .T. ) ;
#11476 = VERTEX_POINT ( 'NONE', #7861 ) ;
#11477 = CARTESIAN_POINT ( 'NONE',  ( -1.988169868018530906, 4.465502636338051445, -13.46874999795161543 ) ) ;
#11478 = DIRECTION ( 'NONE',  ( -0.000000000000000000, -0.000000000000000000, -1.000000000000000000 ) ) ;
#11479 = DIRECTION ( 'NONE',  ( 0.000000000000000000, 0.000000000000000000, 1.000000000000000000 ) ) ;
#11480 = ORIENTED_EDGE ( 'NONE', *, *, #4568, .T. ) ;
#11481 = DIRECTION ( 'NONE',  ( 1.000000000000000000, 0.000000000000000000, 0.000000000000000000 ) ) ;
#11482 = B_SPLINE_CURVE_WITH_KNOTS ( 'NONE', 3,
 ( #8546, #754, #19050, #14458 ),
 .UNSPECIFIED., .F., .F.,
 ( 4, 4 ),
 ( 0.000000000000000000, 0.001126652051248518789 ),
 .UNSPECIFIED. ) ;
#11483 = VERTEX_POINT ( 'NONE', #1771 ) ;
#11484 = DIRECTION ( 'NONE',  ( -1.000000000000000000, -0.000000000000000000, -0.000000000000000000 ) ) ;
#11485 = EDGE_CURVE ( 'NONE', #11735, #17426, #4576, .T. ) ;
#11486 = CONICAL_SURFACE ( 'NONE', #6030, 7.937500000000000000, 1.047197551196596521 ) ;
#11487 = APPLICATION_CONTEXT ( 'automotive_design' ) ;
#11488 = LINE ( 'NONE', #9997, #7723 ) ;
#11489 = CARTESIAN_POINT ( 'NONE',  ( 6.636868745521693924, 5.333637566582140721, -0.3148715423363380173 ) ) ;
#11490 = DIRECTION ( 'NONE',  ( 0.000000000000000000, 0.000000000000000000, 1.000000000000000000 ) ) ;
#11491 = TOROIDAL_SURFACE ( 'NONE', #2856, 24.12539914357697768, 8.000000000000000000 ) ;
#11492 = DIRECTION ( 'NONE',  ( 0.000000000000000000, 0.000000000000000000, 1.000000000000000000 ) ) ;
#11493 = CARTESIAN_POINT ( 'NONE',  ( 18.96448111170889206, 1.130229351527639148, 32.00000000000000000 ) ) ;
#11494 = EDGE_CURVE ( 'NONE', #19430, #4232, #6446, .T. ) ;
#11495 = CARTESIAN_POINT ( 'NONE',  ( -5.476417968967388639, 17.43449690031536292, 32.00000000000000000 ) ) ;
#11496 = ORIENTED_EDGE ( 'NONE', *, *, #13132, .F. ) ;
#11497 = CARTESIAN_POINT ( 'NONE',  ( 112.0000000000000000, 0.000000000000000000, 3.323499999999993015 ) ) ;
#11498 = DIRECTION ( 'NONE',  ( 1.000000000000000000, -0.000000000000000000, 0.000000000000000000 ) ) ;
#11499 = CARTESIAN_POINT ( 'NONE',  ( -1.869200000000000195, 8.279592079675421725E-16, 6.760799999999997034 ) ) ;
#11500 = CARTESIAN_POINT ( 'NONE',  ( 11.34374999795161543, -3.114526743279228072, -3.846120219227966430 ) ) ;
#11501 = CYLINDRICAL_SURFACE ( 'NONE', #17985, 1.000000000000004441 ) ;
#11502 = CARTESIAN_POINT ( 'NONE',  ( 1.773574444220693103, -4.620319390059842490, -7.343749997951615427 ) ) ;
#11503 = VERTEX_POINT ( 'NONE', #12383 ) ;
#11504 = CARTESIAN_POINT ( 'NONE',  ( 2.765633920072239071, -12.59161484032927092, 21.30679549418627161 ) ) ;
#11505 = B_SPLINE_CURVE_WITH_KNOTS ( 'NONE', 3,
 ( #13489, #1096, #7070, #16403, #10108, #5881 ),
 .UNSPECIFIED., .F., .F.,
 ( 4, 2, 4 ),
 ( 2.586195665722962057E-07, 0.001878649493629687504, 0.003757040367692802973 ),
 .UNSPECIFIED. ) ;
#11506 = FACE_OUTER_BOUND ( 'NONE', #6168, .T. ) ;
#11507 = AXIS2_PLACEMENT_3D ( 'NONE', #16745, #8939, #1435 ) ;
#11508 = VERTEX_POINT ( 'NONE', #18476 ) ;
#11509 = ADVANCED_FACE ( 'NONE', ( #6064, #18573 ), #10684, .T. ) ;
#11510 = PRODUCT_DEFINITION ( 'UNKNOWN', '', #12757, #10590 ) ;
#11511 = CARTESIAN_POINT ( 'NONE',  ( 0.000000000000000000, 1.991882183130641248, -24.04302995059964942 ) ) ;
#11512 = DIRECTION ( 'NONE',  ( 0.000000000000000000, -1.224646799147353207E-16, 1.000000000000000000 ) ) ;
#11513 = CARTESIAN_POINT ( 'NONE',  ( 2.783025306068355853, -16.17543236988001354, 18.43727551351025795 ) ) ;
#11514 = ORIENTED_EDGE ( 'NONE', *, *, #9981, .T. ) ;
#11515 = DIRECTION ( 'NONE',  ( -1.000000000000000000, -0.000000000000000000, -0.000000000000000000 ) ) ;
#11516 = CARTESIAN_POINT ( 'NONE',  ( 1.749999999999998002, 0.000000000000000000, 0.000000000000000000 ) ) ;
#11517 = CARTESIAN_POINT ( 'NONE',  ( -8.000000000000000000, 0.000000000000000000, -29.00000000000000000 ) ) ;
#11518 = VERTEX_POINT ( 'NONE', #12581 ) ;
#11519 = EDGE_CURVE ( 'NONE', #17056, #8643, #12231, .T. ) ;
#11520 = CARTESIAN_POINT ( 'NONE',  ( 4.476417968967386862, 17.43449690031536292, 32.00000000000000000 ) ) ;
#11521 = EDGE_LOOP ( 'NONE', ( #19231, #18180, #474, #3704 ) ) ;
#11522 = CIRCLE ( 'NONE', #5112, 1.000000000000000888 ) ;
#11523 = DIRECTION ( 'NONE',  ( 0.000000000000000000, 0.000000000000000000, -1.000000000000000000 ) ) ;
#11524 = CARTESIAN_POINT ( 'NONE',  ( 2.262072769566603636, 24.43806413951692136, -11.57956866523193185 ) ) ;
#11525 = DIRECTION ( 'NONE',  ( 1.000000000000000000, 0.000000000000000000, 0.000000000000000000 ) ) ;
#11526 = DIRECTION ( 'NONE',  ( 0.000000000000000000, -1.000000000000000000, 1.224646799147353207E-16 ) ) ;
#11527 = VERTEX_POINT ( 'NONE', #362 ) ;
#11528 = FACE_BOUND ( 'NONE', #6211, .T. ) ;
#11529 = EDGE_CURVE ( 'NONE', #6632, #3405, #3370, .T. ) ;
#11530 = EDGE_CURVE ( 'NONE', #3019, #8180, #8862, .T. ) ;
#11531 = DIRECTION ( 'NONE',  ( 1.000000000000000000, 0.000000000000000000, 0.000000000000000000 ) ) ;
#11532 = ORIENTED_EDGE ( 'NONE', *, *, #2002, .F. ) ;
#11533 = AXIS2_PLACEMENT_3D ( 'NONE', #1102, #998, #5588 ) ;
#11534 = EDGE_CURVE ( 'NONE', #9486, #2268, #10137, .T. ) ;
#11535 = DIRECTION ( 'NONE',  ( -1.000000000000000000, 0.000000000000000000, -0.000000000000000000 ) ) ;
#11536 = CARTESIAN_POINT ( 'NONE',  ( -1.510506337161893642, -4.648860486681943627, -12.84374999795161543 ) ) ;
#11537 = ORIENTED_EDGE ( 'NONE', *, *, #13571, .F. ) ;
#11538 = CARTESIAN_POINT ( 'NONE',  ( 0.006931111373680289185, 9.685942809247373830, -22.53293026234493723 ) ) ;
#11539 = CARTESIAN_POINT ( 'NONE',  ( -3.499494075959840078, -3.499494075959792116, -13.96874999795161365 ) ) ;
#11540 = CARTESIAN_POINT ( 'NONE',  ( 14.86923836996420434, -11.47363181547641453, 32.00000000000000000 ) ) ;
#11541 = VERTEX_POINT ( 'NONE', #9183 ) ;
#11542 = DIRECTION ( 'NONE',  ( 0.000000000000000000, 1.000000000000000000, -0.000000000000000000 ) ) ;
#11543 = ORIENTED_EDGE ( 'NONE', *, *, #4801, .F. ) ;
#11544 = ITEM_DEFINED_TRANSFORMATION ( 'NONE', 'NONE', #3161,  #16724 ) ;
#11545 = CARTESIAN_POINT ( 'NONE',  ( -11.00000000000000355, -3.278623949159158446, -2.625000000000002220 ) ) ;
#11546 = FACE_OUTER_BOUND ( 'NONE', #2191, .T. ) ;
#11547 = LINE ( 'NONE', #17653, #11556 ) ;
#11548 = ORIENTED_EDGE ( 'NONE', *, *, #3825, .F. ) ;
#11549 =( BOUNDED_CURVE ( )  B_SPLINE_CURVE ( 2, ( #16908, #1888, #18789, #4892, #7788, #3392, #1696, #12795, #7880 ),
 .UNSPECIFIED., .F., .F. ) 
 B_SPLINE_CURVE_WITH_KNOTS ( ( 3, 2, 2, 2, 3 ),
 ( 0.000000000000000000, 0.05000000000000000278, 0.1000000000000000056, 0.1499999999999999944, 0.1666819079834106210 ),
 .UNSPECIFIED. ) 
 CURVE ( )  GEOMETRIC_REPRESENTATION_ITEM ( )  RATIONAL_B_SPLINE_CURVE ( ( 1.000000000000000000, 0.9876883405951377704, 1.000000000000000000, 0.9876883405951377704, 1.000000000000000000, 0.9876883405951377704, 1.000000000000000000, 0.9958923606136999007, 0.9945256517182514688 ) ) 
 REPRESENTATION_ITEM ( '' )  );
#11550 = DIRECTION ( 'NONE',  ( 0.000000000000000000, 0.000000000000000000, -1.000000000000000000 ) ) ;
#11551 = CARTESIAN_POINT ( 'NONE',  ( -3.255998204157480203, -17.85806462366060288, 35.00000000000000000 ) ) ;
#11552 = AXIS2_PLACEMENT_3D ( 'NONE', #7425, #1743, #16763 ) ;
#11553 = AXIS2_PLACEMENT_3D ( 'NONE', #14337, #5120, #8439 ) ;
#11554 = DIRECTION ( 'NONE',  ( -1.000000000000000000, -0.000000000000000000, -0.000000000000000000 ) ) ;
#11555 = ORIENTED_EDGE ( 'NONE', *, *, #1863, .F. ) ;
#11556 = VECTOR ( 'NONE', #14657, 1000.000000000000000 ) ;
#11557 = CARTESIAN_POINT ( 'NONE',  ( -5.294050593750000644, 0.000000000000000000, -6.234374998975811266 ) ) ;
#11558 = EDGE_LOOP ( 'NONE', ( #3912, #775, #11837, #19234 ) ) ;
#11559 = CIRCLE ( 'NONE', #15077, 0.9999999999999974465 ) ;
#11560 = AXIS2_PLACEMENT_3D ( 'NONE', #5976, #7269, #19393 ) ;
#11561 = DIRECTION ( 'NONE',  ( 0.000000000000000000, 0.000000000000000000, -1.000000000000000000 ) ) ;
#11562 = VECTOR ( 'NONE', #4018, 1000.000000000000000 ) ;
#11563 = DIRECTION ( 'NONE',  ( 1.000000000000000000, 0.000000000000000000, 0.000000000000000000 ) ) ;
#11564 = ORIENTED_EDGE ( 'NONE', *, *, #263, .T. ) ;
#11565 = CARTESIAN_POINT ( 'NONE',  ( -2.695436003842674566, 4.150607464521828938, -12.96874999795161543 ) ) ;
#11566 = CARTESIAN_POINT ( 'NONE',  ( -1.773574444220725077, 4.620319390059829168, -6.968749997951614539 ) ) ;
#11567 = AXIS2_PLACEMENT_3D ( 'NONE', #10194, #18996, #15995 ) ;
#11568 = EDGE_LOOP ( 'NONE', ( #556, #12676 ) ) ;
#11569 = ORIENTED_EDGE ( 'NONE', *, *, #17176, .T. ) ;
#11570 = CARTESIAN_POINT ( 'NONE',  ( -3.270778111535288080, 3.632567103900569361, -12.46874999795161543 ) ) ;
#11571 = DIRECTION ( 'NONE',  ( 0.000000000000000000, 0.000000000000000000, -1.000000000000000000 ) ) ;
#11572 = AXIS2_PLACEMENT_3D ( 'NONE', #9706, #4986, #13999 ) ;
#11573 = CARTESIAN_POINT ( 'NONE',  ( -4.762500000000000178, 0.000000000000000000, -6.502399999999998847 ) ) ;
#11574 = VECTOR ( 'NONE', #5073, 1000.000000000000000 ) ;
#11575 = ORIENTED_EDGE ( 'NONE', *, *, #18526, .F. ) ;
#11576 = DIRECTION ( 'NONE',  ( 0.000000000000000000, 1.374038396813314756E-15, -1.000000000000000000 ) ) ;
#11577 = AXIS2_PLACEMENT_3D ( 'NONE', #6879, #12711, #17212 ) ;
#11578 = LINE ( 'NONE', #18080, #6259 ) ;
#11579 = ORIENTED_EDGE ( 'NONE', *, *, #14767, .T. ) ;
#11580 = DIRECTION ( 'NONE',  ( 0.000000000000000000, 0.000000000000000000, 1.000000000000000000 ) ) ;
#11581 = EDGE_CURVE ( 'NONE', #126, #14843, #4770, .T. ) ;
#11582 = AXIS2_PLACEMENT_3D ( 'NONE', #16493, #73, #16690 ) ;
#11583 = DIRECTION ( 'NONE',  ( 0.000000000000000000, 0.000000000000000000, -1.000000000000000000 ) ) ;
#11584 = CARTESIAN_POINT ( 'NONE',  ( 4.643890550183617627, 6.484284064149637317, -0.01675691374232827352 ) ) ;
#11585 = CARTESIAN_POINT ( 'NONE',  ( 12.34374999795161543, -1.773574444220693325, -4.620319390059842490 ) ) ;
#11586 = CIRCLE ( 'NONE', #19251, 1.000000000000000888 ) ;
#11587 = EDGE_CURVE ( 'NONE', #14330, #4430, #15578, .T. ) ;
#11588 = FACE_OUTER_BOUND ( 'NONE', #14409, .T. ) ;
#11589 = CARTESIAN_POINT ( 'NONE',  ( 2.783025336474041378, -12.53640742967737332, -21.08118142846917209 ) ) ;
#11590 = CIRCLE ( 'NONE', #5514, 1.000000000000004441 ) ;
#11591 = ORIENTED_EDGE ( 'NONE', *, *, #4757, .F. ) ;
#11592 = DIRECTION ( 'NONE',  ( -1.000000000000000000, 0.000000000000000000, 0.000000000000000000 ) ) ;
#11593 = FACE_OUTER_BOUND ( 'NONE', #11894, .T. ) ;
#11594 = CLOSED_SHELL ( 'NONE', ( #9333, #16263, #10451, #18464, #17123, #15041 ) ) ;
#11595 = UNCERTAINTY_MEASURE_WITH_UNIT (LENGTH_MEASURE( 1.000000000000000082E-05 ), #4650, 'distance_accuracy_value', 'NONE');
#11596 = CARTESIAN_POINT ( 'NONE',  ( 5.575441324182689229, -1.185096637661254171, -11.31249999590322375 ) ) ;
#11597 = CARTESIAN_POINT ( 'NONE',  ( 2.624330855611206381, -7.650277397455553796, -0.08160424337825018803 ) ) ;
#11598 = CARTESIAN_POINT ( 'NONE',  ( -3.350375938067097437, 4.611396867937201272, -10.31249999590322552 ) ) ;
#11599 = VERTEX_POINT ( 'NONE', #10977 ) ;
#11600 = DIRECTION ( 'NONE',  ( 0.000000000000000000, 0.000000000000000000, -1.000000000000000000 ) ) ;
#11601 = CARTESIAN_POINT ( 'NONE',  ( 8.000000000000000000, 9.797174393178825657E-16, -29.00000000000000000 ) ) ;
#11602 = ORIENTED_EDGE ( 'NONE', *, *, #14642, .T. ) ;
#11603 = CARTESIAN_POINT ( 'NONE',  ( 6.000000000000005329, 4.936344801571289409, 2.850000000000024070 ) ) ;
#11604 = EDGE_CURVE ( 'NONE', #6062, #11862, #10453, .T. ) ;
#11605 = CARTESIAN_POINT ( 'NONE',  ( 0.02436607992776064838, 5.391175441198615914, 24.15498966839965078 ) ) ;
#11606 = AXIS2_PLACEMENT_3D ( 'NONE', #9229, #13625, #18040 ) ;
#11607 = AXIS2_PLACEMENT_3D ( 'NONE', #4608, #5994, #1707 ) ;
#11608 = CARTESIAN_POINT ( 'NONE',  ( 7.312499995903225525, 0.000000000000000000, -5.700000000000001066 ) ) ;
#11609 = DIRECTION ( 'NONE',  ( 0.000000000000000000, 0.000000000000000000, 1.000000000000000000 ) ) ;
#11610 = ORIENTED_EDGE ( 'NONE', *, *, #11657, .T. ) ;
#11611 = LINE ( 'NONE', #9736, #13616 ) ;
#11612 = CARTESIAN_POINT ( 'NONE',  ( 17.96448111170888851, 1.130229351527639148, 32.00000000000000000 ) ) ;
#11613 = DIRECTION ( 'NONE',  ( 0.000000000000000000, 0.000000000000000000, 1.000000000000000000 ) ) ;
#11614 = VERTEX_POINT ( 'NONE', #10877 ) ;
#11615 = DIRECTION ( 'NONE',  ( -1.000000000000000000, -0.000000000000000000, -0.000000000000000000 ) ) ;
#11616 = ORIENTED_EDGE ( 'NONE', *, *, #4757, .T. ) ;
#11617 = CARTESIAN_POINT ( 'NONE',  ( 7.937499999999996447, -4.582717761692668645, -0.7089489049740167470 ) ) ;
#11618 = DIRECTION ( 'NONE',  ( 0.000000000000000000, 0.000000000000000000, -1.000000000000000000 ) ) ;
#11619 = EDGE_CURVE ( 'NONE', #4430, #12789, #6165, .T. ) ;
#11620 = DIRECTION ( 'NONE',  ( 0.000000000000000000, 0.000000000000000000, 1.000000000000000000 ) ) ;
#11621 = EDGE_CURVE ( 'NONE', #13895, #4324, #4060, .T. ) ;
#11622 = CARTESIAN_POINT ( 'NONE',  ( -0.5109457054261112852, 4.861323657744413218, -14.84374999795161543 ) ) ;
#11623 = ORIENTED_EDGE ( 'NONE', *, *, #19029, .F. ) ;
#11624 = VECTOR ( 'NONE', #3808, 1000.000000000000000 ) ;
#11625 = CARTESIAN_POINT ( 'NONE',  ( 4.500000000000000000, 5.510910596163088569E-16, -35.00000000000000000 ) ) ;
#11626 = EDGE_CURVE ( 'NONE', #9660, #2276, #17167, .T. ) ;
#11627 = ORIENTED_EDGE ( 'NONE', *, *, #10919, .F. ) ;
#11628 = EDGE_CURVE ( 'NONE', #8576, #11336, #19707, .T. ) ;
#11629 =( GEOMETRIC_REPRESENTATION_CONTEXT ( 3 ) GLOBAL_UNCERTAINTY_ASSIGNED_CONTEXT ( ( #11401 ) ) GLOBAL_UNIT_ASSIGNED_CONTEXT ( ( #9686, #3170, #9483 ) ) REPRESENTATION_CONTEXT ( 'NONE', 'WORKASPACE' ) );
#11630 = CIRCLE ( 'NONE', #17746, 24.12539914357697768 ) ;
#11631 = CYLINDRICAL_SURFACE ( 'NONE', #12203, 13.19999999999999929 ) ;
#11632 = DIRECTION ( 'NONE',  ( 0.000000000000000000, 0.000000000000000000, -1.000000000000000000 ) ) ;
#11633 = ORIENTED_EDGE ( 'NONE', *, *, #18860, .T. ) ;
#11634 = CARTESIAN_POINT ( 'NONE',  ( -7.937500000000000000, -3.073999505363502749, -0.3133235625263136037 ) ) ;
#11635 = CARTESIAN_POINT ( 'NONE',  ( 2.873153789725797491, -3.954556930911881985, -9.468749997951615427 ) ) ;
#11636 = FACE_BOUND ( 'NONE', #19142, .T. ) ;
#11637 = TOROIDAL_SURFACE ( 'NONE', #7787, 24.12539914357697413, 8.000000000000000000 ) ;
#11638 = VERTEX_POINT ( 'NONE', #15384 ) ;
#11639 = DIRECTION ( 'NONE',  ( -1.000000000000000000, -0.000000000000000000, -0.000000000000000000 ) ) ;
#11640 = DIRECTION ( 'NONE',  ( 1.000000000000000000, 0.000000000000000000, 0.000000000000000000 ) ) ;
#11641 = EDGE_LOOP ( 'NONE', ( #3051, #1233, #15649, #16333 ) ) ;
#11642 = FACE_OUTER_BOUND ( 'NONE', #1086, .T. ) ;
#11643 = PLANE ( 'NONE',  #16668 ) ;
#11644 = VERTEX_POINT ( 'NONE', #9383 ) ;
#11645 = CARTESIAN_POINT ( 'NONE',  ( 1.749999999999998002, -19.67366047555544739, 20.02152543075338897 ) ) ;
#11646 = CARTESIAN_POINT ( 'NONE',  ( 8.812499995903225525, -2.620002426024580000, 5.142044285764733935 ) ) ;
#11647 = CIRCLE ( 'NONE', #6515, 24.12539914357697413 ) ;
#11648 = CYLINDRICAL_SURFACE ( 'NONE', #19722, 6.000000000000000000 ) ;
#11649 = EDGE_CURVE ( 'NONE', #19556, #19358, #11087, .T. ) ;
#11650 = ORIENTED_EDGE ( 'NONE', *, *, #19364, .F. ) ;
#11651 = CARTESIAN_POINT ( 'NONE',  ( 6.843749997951615427, 0.000000000000000000, -4.888101187500000222 ) ) ;
#11652 = AXIS2_PLACEMENT_3D ( 'NONE', #18021, #5789, #13704 ) ;
#11653 = EDGE_CURVE ( 'NONE', #10856, #7344, #18872, .T. ) ;
#11654 = ADVANCED_FACE ( 'NONE', ( #12776 ), #5346, .T. ) ;
#11655 = VERTEX_POINT ( 'NONE', #3468 ) ;
#11656 = DIRECTION ( 'NONE',  ( 1.000000000000000000, 0.000000000000000000, 0.000000000000000000 ) ) ;
#11657 = EDGE_CURVE ( 'NONE', #3117, #8877, #13645, .T. ) ;
#11658 = CARTESIAN_POINT ( 'NONE',  ( 112.0000000000000000, 4.000000000000000000, 0.000000000000000000 ) ) ;
#11659 = ORIENTED_EDGE ( 'NONE', *, *, #2355, .T. ) ;
#11660 =( BOUNDED_CURVE ( )  B_SPLINE_CURVE ( 2, ( #17175, #3464, #3260, #12771, #6441, #11269, #571, #6643, #7856, #12577, #9574, #1959, #5150, #10972, #17076 ),
 .UNSPECIFIED., .F., .F. ) 
 B_SPLINE_CURVE_WITH_KNOTS ( ( 3, 2, 2, 2, 2, 2, 2, 3 ),
 ( 0.000000000000000000, 0.05000000000000000278, 0.1000000000000000056, 0.1499999999999999944, 0.2000000000000000111, 0.2500000000000000000, 0.2999999999999999889, 0.3333180920165860761 ),
 .UNSPECIFIED. ) 
 CURVE ( )  GEOMETRIC_REPRESENTATION_ITEM ( )  RATIONAL_B_SPLINE_CURVE ( ( 1.000000000000000000, 0.9876883405951377704, 1.000000000000000000, 0.9876883405951377704, 1.000000000000000000, 0.9876883405951377704, 1.000000000000000000, 0.9876883405951377704, 1.000000000000000000, 0.9876883405951377704, 1.000000000000000000, 0.9876883405951377704, 1.000000000000000000, 0.9917959799814386468, 0.9945256517182510247 ) ) 
 REPRESENTATION_ITEM ( '' )  );
#11661 = CARTESIAN_POINT ( 'NONE',  ( -4.861323657744413218, -0.5109457054261099529, -9.468749997951615427 ) ) ;
#11662 = DIRECTION ( 'NONE',  ( -1.000000000000000000, 0.000000000000000000, 0.000000000000000000 ) ) ;
#11663 = ORIENTED_EDGE ( 'NONE', *, *, #12335, .T. ) ;
#11664 = VERTEX_POINT ( 'NONE', #16341 ) ;
#11665 = CARTESIAN_POINT ( 'NONE',  ( 8.671566133830875600, 15.77352024078954784, -32.00000000000000000 ) ) ;
#11666 = EDGE_CURVE ( 'NONE', #3037, #9666, #674, .T. ) ;
#11667 = CARTESIAN_POINT ( 'NONE',  ( 7.468749997951615427, 3.270778111535313837, 3.632567103900546712 ) ) ;
#11668 = EDGE_CURVE ( 'NONE', #11599, #4605, #8059, .T. ) ;
#11669 = ORIENTED_EDGE ( 'NONE', *, *, #5159, .F. ) ;
#11670 = AXIS2_PLACEMENT_3D ( 'NONE', #12963, #15963, #855 ) ;
#11671 = CARTESIAN_POINT ( 'NONE',  ( 14.19790265903627180, 9.644882309621939598, -32.00000000000000000 ) ) ;
#11672 = AXIS2_PLACEMENT_3D ( 'NONE', #8083, #18891, #18593 ) ;
#11673 = VERTEX_POINT ( 'NONE', #12678 ) ;
#11674 = CARTESIAN_POINT ( 'NONE',  ( 0.5958122406255995651, -5.668774803599162304, -15.31249999590322552 ) ) ;
#11675 = CARTESIAN_POINT ( 'NONE',  ( 13.00000000000000533, -4.057257337410487885, 2.726922038711669494 ) ) ;
#11676 = VERTEX_POINT ( 'NONE', #1964 ) ;
#11677 = DIRECTION ( 'NONE',  ( 1.000000000000000000, 6.419766481290786633E-33, -0.000000000000000000 ) ) ;
#11678 = LINE ( 'NONE', #17786, #9340 ) ;
#11679 = EDGE_CURVE ( 'NONE', #4468, #9544, #1189, .T. ) ;
#11680 = CARTESIAN_POINT ( 'NONE',  ( 7.937500000000000000, 4.582717761692664205, -0.7089489049740167470 ) ) ;
#11681 = DIRECTION ( 'NONE',  ( -1.000000000000000000, -0.000000000000000000, -0.000000000000000000 ) ) ;
#11682 = AXIS2_PLACEMENT_3D ( 'NONE', #28, #14131, #4829 ) ;
#11683 = DIRECTION ( 'NONE',  ( 0.000000000000000000, 0.000000000000000000, -1.000000000000000000 ) ) ;
#11684 = CYLINDRICAL_SURFACE ( 'NONE', #8386, 13.19999999999999929 ) ;
#11685 = VECTOR ( 'NONE', #11479, 1000.000000000000000 ) ;
#11686 = ORIENTED_EDGE ( 'NONE', *, *, #1103, .F. ) ;
#11687 = B_SPLINE_CURVE_WITH_KNOTS ( 'NONE', 3,
 ( #7092, #19124, #8713, #13031, #19312, #11338 ),
 .UNSPECIFIED., .F., .F.,
 ( 4, 2, 4 ),
 ( 1.979325885420528755E-07, 0.001878588715165608204, 0.003756979497742674035 ),
 .UNSPECIFIED. ) ;
#11688 = DIRECTION ( 'NONE',  ( -1.000000000000000000, 0.000000000000000000, 0.000000000000000000 ) ) ;
#11689 = EDGE_CURVE ( 'NONE', #16591, #4589, #1282, .T. ) ;
#11690 = CARTESIAN_POINT ( 'NONE',  ( 1.000000000000003331, 18.00000000000000355, 32.00000000000000000 ) ) ;
#11691 = FACE_OUTER_BOUND ( 'NONE', #10223, .T. ) ;
#11692 = EDGE_CURVE ( 'NONE', #3073, #17337, #16207, .T. ) ;
#11693 = CARTESIAN_POINT ( 'NONE',  ( 2.695436003842704764, -4.150607464521811174, -12.96874999795161543 ) ) ;
#11694 = CARTESIAN_POINT ( 'NONE',  ( -4.942249507334558700, -0.2590123213420630899, -13.34374999795161365 ) ) ;
#11695 = VERTEX_POINT ( 'NONE', #17743 ) ;
#11696 = LINE ( 'NONE', #16210, #19225 ) ;
#11697 = AXIS2_PLACEMENT_3D ( 'NONE', #18426, #1724, #7814 ) ;
#11698 = ORIENTED_EDGE ( 'NONE', *, *, #14856, .T. ) ;
#11699 = DIRECTION ( 'NONE',  ( 0.000000000000000000, 0.000000000000000000, -1.000000000000000000 ) ) ;
#11700 = ADVANCED_FACE ( 'NONE', ( #4039 ), #576, .T. ) ;
#11701 = TOROIDAL_SURFACE ( 'NONE', #5619, 24.12539914357697413, 8.000000000000000000 ) ;
#11702 = DIRECTION ( 'NONE',  ( 0.000000000000000000, 0.000000000000000000, 1.000000000000000000 ) ) ;
#11703 = DIRECTION ( 'NONE',  ( 0.000000000000000000, -1.000000000000000000, -4.122115190439943875E-15 ) ) ;
#11704 = DIRECTION ( 'NONE',  ( -1.000000000000000000, -0.000000000000000000, -0.000000000000000000 ) ) ;
#11705 = ORIENTED_EDGE ( 'NONE', *, *, #4899, .F. ) ;
#11706 = CARTESIAN_POINT ( 'NONE',  ( 2.765633920072235075, 24.63872515616082737, -2.336989772644355590 ) ) ;
#11707 =( NAMED_UNIT ( * ) PLANE_ANGLE_UNIT ( ) SI_UNIT ( $, .RADIAN. ) );
#11708 = DIRECTION ( 'NONE',  ( 1.000000000000000000, 0.000000000000000000, 0.000000000000000000 ) ) ;
#11709 = CARTESIAN_POINT ( 'NONE',  ( 12.50000000000000533, -5.142044285764733935, -2.620002426024580000 ) ) ;
#11710 = VERTEX_POINT ( 'NONE', #2062 ) ;
#11711 = B_SPLINE_CURVE_WITH_KNOTS ( 'NONE', 1,
 ( #5563, #11674 ),
 .UNSPECIFIED., .F., .F.,
 ( 2, 2 ),
 ( 0.000000000000000000, 1.000000000000000000 ),
 .UNSPECIFIED. ) ;
#11712 = DIRECTION ( 'NONE',  ( 0.000000000000000000, 0.000000000000000000, 1.000000000000000000 ) ) ;
#11713 = AXIS2_PLACEMENT_3D ( 'NONE', #18498, #12605, #13801 ) ;
#11714 = ORIENTED_EDGE ( 'NONE', *, *, #12523, .T. ) ;
#11715 = CARTESIAN_POINT ( 'NONE',  ( 0.1855654851361731306, -10.67816411292181655, 23.63475234378979195 ) ) ;
#11716 = ADVANCED_FACE ( 'NONE', ( #10148 ), #14745, .T. ) ;
#11717 = AXIS2_PLACEMENT_3D ( 'NONE', #9923, #13295, #16010 ) ;
#11718 = CYLINDRICAL_SURFACE ( 'NONE', #16522, 4.400000000000000355 ) ;
#11719 = CARTESIAN_POINT ( 'NONE',  ( -3.954556930911881096, -2.873153789725797935, -14.46874999795161720 ) ) ;
#11720 = CARTESIAN_POINT ( 'NONE',  ( -4.080749450109650844, 4.080749450109650844, -8.500000000000005329 ) ) ;
#11721 = ORIENTED_EDGE ( 'NONE', *, *, #1055, .F. ) ;
#11722 = CARTESIAN_POINT ( 'NONE',  ( 1.773574444220693103, -4.620319390059841602, -6.968749997951614539 ) ) ;
#11723 = DIRECTION ( 'NONE',  ( -1.000000000000000000, -0.000000000000000000, -0.000000000000000000 ) ) ;
#11724 = EDGE_LOOP ( 'NONE', ( #4416, #7452, #2697, #12988, #520, #1551, #19504 ) ) ;
#11725 = AXIS2_PLACEMENT_3D ( 'NONE', #13334, #14374, #2163 ) ;
#11726 = EDGE_CURVE ( 'NONE', #11007, #8766, #3099, .T. ) ;
#11727 = AXIS2_PLACEMENT_3D ( 'NONE', #2411, #11618, #13124 ) ;
#11728 = DIRECTION ( 'NONE',  ( -1.000000000000000000, 1.224646799147353207E-16, 0.000000000000000000 ) ) ;
#11729 = EDGE_CURVE ( 'NONE', #10630, #12192, #18675, .T. ) ;
#11730 = CARTESIAN_POINT ( 'NONE',  ( -2.873153789725852558, -3.954556930911842016, -13.84374999795161543 ) ) ;
#11731 = EDGE_LOOP ( 'NONE', ( #9577, #11475, #17214, #14315 ) ) ;
#11732 = CARTESIAN_POINT ( 'NONE',  ( -2.444050593749990341, 4.233219804643887585, -6.843749997951615427 ) ) ;
#11733 = PLANE ( 'NONE',  #19362 ) ;
#11734 = CARTESIAN_POINT ( 'NONE',  ( 8.968749997951613651, 3.499494075959816541, -3.499494075959816541 ) ) ;
#11735 = VERTEX_POINT ( 'NONE', #17180 ) ;
#11736 = CARTESIAN_POINT ( 'NONE',  ( 1.000000000000003331, 18.00000000000000355, -35.00000000000000000 ) ) ;
#11737 = ORIENTED_EDGE ( 'NONE', *, *, #3560, .T. ) ;
#11738 = DIRECTION ( 'NONE',  ( 0.000000000000000000, 0.000000000000000000, -1.000000000000000000 ) ) ;
#11739 = ORIENTED_EDGE ( 'NONE', *, *, #2889, .T. ) ;
#11740 = CARTESIAN_POINT ( 'NONE',  ( 8.968749997951611874, 1.280903732194421218, 4.780397808154266848 ) ) ;
#11741 = DIRECTION ( 'NONE',  ( -1.000000000000000000, 0.000000000000000000, 0.000000000000000000 ) ) ;
#11742 = EDGE_CURVE ( 'NONE', #18451, #7112, #9685, .T. ) ;
#11743 = EDGE_CURVE ( 'NONE', #10395, #6118, #3562, .T. ) ;
#11744 = CYLINDRICAL_SURFACE ( 'NONE', #1318, 13.19999999999999929 ) ;
#11745 = DIRECTION ( 'NONE',  ( 1.000000000000000000, 0.000000000000000000, 0.000000000000000000 ) ) ;
#11746 = CARTESIAN_POINT ( 'NONE',  ( 9.500000000000003553, -4.840010801796461593, -3.143139765844656708 ) ) ;
#11747 = AXIS2_PLACEMENT_3D ( 'NONE', #4209, #6090, #2796 ) ;
#11748 = CYLINDRICAL_SURFACE ( 'NONE', #4078, 6.000000000000000888 ) ;
#11749 = VECTOR ( 'NONE', #17364, 1000.000000000000000 ) ;
#11750 = EDGE_LOOP ( 'NONE', ( #1095, #5728 ) ) ;
#11751 = CARTESIAN_POINT ( 'NONE',  ( 11.32184790671639263, 13.12143529358541016, -32.00000000000000000 ) ) ;
#11752 = VERTEX_POINT ( 'NONE', #14275 ) ;
#11753 = B_SPLINE_CURVE_WITH_KNOTS ( 'NONE', 3,
 ( #3140, #239, #15259, #15357 ),
 .UNSPECIFIED., .F., .F.,
 ( 4, 4 ),
 ( 0.005258139959819225183, 0.005948405594583413246 ),
 .UNSPECIFIED. ) ;
#11754 = CYLINDRICAL_SURFACE ( 'NONE', #9646, 1.000000000000004441 ) ;
#11755 = DIRECTION ( 'NONE',  ( 0.000000000000000000, 0.000000000000000000, 1.000000000000000000 ) ) ;
#11756 = DIRECTION ( 'NONE',  ( 0.000000000000000000, 0.5000000000000039968, -0.8660254037844363761 ) ) ;
#11757 = AXIS2_PLACEMENT_3D ( 'NONE', #15045, #18149, #4732 ) ;
#11758 = DIRECTION ( 'NONE',  ( 1.000000000000000000, 0.000000000000000000, 0.000000000000000000 ) ) ;
#11759 = ORIENTED_EDGE ( 'NONE', *, *, #18562, .T. ) ;
#11760 = FACE_OUTER_BOUND ( 'NONE', #9606, .T. ) ;
#11761 = DIRECTION ( 'NONE',  ( 0.000000000000000000, 0.000000000000000000, 1.000000000000000000 ) ) ;
#11762 = CARTESIAN_POINT ( 'NONE',  ( 2.647025296874957689, -4.584782303107616031, -6.234374998975811266 ) ) ;
#11763 = EDGE_CURVE ( 'NONE', #10072, #8830, #7929, .T. ) ;
#11764 = ORIENTED_EDGE ( 'NONE', *, *, #16940, .T. ) ;
#11765 = VERTEX_POINT ( 'NONE', #16845 ) ;
#11766 = ADVANCED_FACE ( 'NONE', ( #9034 ), #13008, .T. ) ;
#11767 = DIRECTION ( 'NONE',  ( 0.000000000000000000, 0.000000000000000000, -1.000000000000000000 ) ) ;
#11768 = CARTESIAN_POINT ( 'NONE',  ( -90.00000000000000000, 0.000000000000000000, 0.000000000000000000 ) ) ;
#11769 = ORIENTED_EDGE ( 'NONE', *, *, #18131, .T. ) ;
#11770 = AXIS2_PLACEMENT_3D ( 'NONE', #1968, #17085, #9488 ) ;
#11771 = CARTESIAN_POINT ( 'NONE',  ( 5.387740456496233676, 2.068159791354183596, -11.50000000000000355 ) ) ;
#11772 = ORIENTED_EDGE ( 'NONE', *, *, #18962, .T. ) ;
#11773 = DIRECTION ( 'NONE',  ( 1.000000000000000000, 0.000000000000000000, 0.000000000000000000 ) ) ;
#11774 = EDGE_CURVE ( 'NONE', #16239, #18193, #3124, .T. ) ;
#11775 = CARTESIAN_POINT ( 'NONE',  ( 13.00000000000000888, -4.471046188018891421, -1.976722499206046146 ) ) ;
#11776 = ORIENTED_EDGE ( 'NONE', *, *, #17717, .F. ) ;
#11777 = LINE ( 'NONE', #10385, #1137 ) ;
#11778 =( BOUNDED_SURFACE ( )  B_SPLINE_SURFACE ( 1, 2, ( 
 ( #400, #14102, #4802, #17207, #17014, #3302, #12706, #11104, #9415, #3499, #6479, #12613, #16825, #13910, #15610, #18603, #509 ),
 ( #9609, #6577, #18801, #10714, #15513, #9216, #1800, #3101, #7893, #105, #14009, #18410, #6379, #4704, #10811, #7798, #12510 ) ),
 .UNSPECIFIED., .F., .F., .F. ) 
 B_SPLINE_SURFACE_WITH_KNOTS ( ( 2, 2 ),
 ( 3, 2, 2, 2, 2, 2, 2, 2, 3 ),
 ( 0.000000000000000000, 1.000000000000000000 ),
 ( 0.000000000000000000, 0.05000000000000000278, 0.1000000000000000056, 0.1499999999999999944, 0.2000000000000000111, 0.2500000000000000000, 0.2999999999999999889, 0.3499999999999999778, 0.4000000000000000222 ),
 .UNSPECIFIED. ) 
 GEOMETRIC_REPRESENTATION_ITEM ( )  RATIONAL_B_SPLINE_SURFACE ( (
 ( 1.000000000000000000, 0.9876883405951377704, 1.000000000000000000, 0.9876883405951377704, 1.000000000000000000, 0.9876883405951377704, 1.000000000000000000, 0.9876883405951377704, 1.000000000000000000, 0.9876883405951377704, 1.000000000000000000, 0.9876883405951377704, 1.000000000000000000, 0.9876883405951377704, 1.000000000000000000, 0.9876883405951377704, 1.000000000000000000),
 ( 1.000000000000000000, 0.9876883405951377704, 1.000000000000000000, 0.9876883405951377704, 1.000000000000000000, 0.9876883405951377704, 1.000000000000000000, 0.9876883405951377704, 1.000000000000000000, 0.9876883405951377704, 1.000000000000000000, 0.9876883405951377704, 1.000000000000000000, 0.9876883405951377704, 1.000000000000000000, 0.9876883405951377704, 1.000000000000000000) ) ) 
 REPRESENTATION_ITEM ( '' )  SURFACE ( )  );
#11780 = EDGE_CURVE ( 'NONE', #2009, #3616, #12375, .T. ) ;
#11779 = EDGE_CURVE ( 'NONE', #2901, #2678, #8214, .T. ) ;
#11781 = CARTESIAN_POINT ( 'NONE',  ( -10.00000000000000000, 0.000000000000000000, 0.000000000000000000 ) ) ;
#11782 = CARTESIAN_POINT ( 'NONE',  ( 2.789999999999999147, 5.535312321043049266, -23.48180575137724446 ) ) ;
#11783 = PRODUCT_DEFINITION_SHAPE ( 'NONE', 'NONE',  #10899 ) ;
#11784 = AXIS2_PLACEMENT_3D ( 'NONE', #17847, #17948, #8550 ) ;
#11785 = CARTESIAN_POINT ( 'NONE',  ( -2.000000000000000000, -5.000000000000001776, 41.99999999999999289 ) ) ;
#11786 = FILL_AREA_STYLE_COLOUR ( '', #10358 ) ;
#11787 = DIRECTION ( 'NONE',  ( 1.000000000000000000, 0.000000000000000000, 0.000000000000000000 ) ) ;
#11788 = EDGE_LOOP ( 'NONE', ( #12961, #2474, #11398, #6901 ) ) ;
#11789 = CARTESIAN_POINT ( 'NONE',  ( 1.999999999999999112, 0.000000000000000000, -4.200000000000000178 ) ) ;
#11790 = CARTESIAN_POINT ( 'NONE',  ( -10.00000000000000000, 0.000000000000000000, 0.000000000000000000 ) ) ;
#11791 = B_SPLINE_CURVE_WITH_KNOTS ( 'NONE', 1,
 ( #16322, #12015 ),
 .UNSPECIFIED., .F., .F.,
 ( 2, 2 ),
 ( 0.000000000000000000, 1.000000000000000000 ),
 .UNSPECIFIED. ) ;
#11792 = UNCERTAINTY_MEASURE_WITH_UNIT (LENGTH_MEASURE( 1.000000000000000082E-05 ), #9933, 'distance_accuracy_value', 'NONE');
#11793 = FACE_OUTER_BOUND ( 'NONE', #824, .T. ) ;
#11794 = DIRECTION ( 'NONE',  ( 0.000000000000000000, 0.000000000000000000, 1.000000000000000000 ) ) ;
#11795 = CARTESIAN_POINT ( 'NONE',  ( 0.02436607992776151574, 24.15498966839970052, -5.391175441198366336 ) ) ;
#11796 = EDGE_LOOP ( 'NONE', ( #19121, #17403 ) ) ;
#11797 = LINE ( 'NONE', #4097, #17951 ) ;
#11798 = DIRECTION ( 'NONE',  ( 0.000000000000000000, -1.000000000000000000, 0.000000000000000000 ) ) ;
#11799 = ORIENTED_EDGE ( 'NONE', *, *, #9619, .T. ) ;
#11800 = CARTESIAN_POINT ( 'NONE',  ( 6.843749997951615427, 4.233219804643871598, 2.444050593750020095 ) ) ;
#11801 = DIRECTION ( 'NONE',  ( -0.4999999999999978351, -0.7499999999999990008, -0.4330127018922234616 ) ) ;
#11802 = STYLED_ITEM ( 'NONE', ( #7021 ), #16178 ) ;
#11803 = B_SPLINE_CURVE_WITH_KNOTS ( 'NONE', 3,
 ( #10291, #16387, #17591, #3879, #8581, #19379 ),
 .UNSPECIFIED., .F., .F.,
 ( 4, 2, 4 ),
 ( 4.462636678113234028E-07, 0.001879885020955180275, 0.003759323778242549142 ),
 .UNSPECIFIED. ) ;
#11804 = DIRECTION ( 'NONE',  ( -0.000000000000000000, -0.000000000000000000, 1.000000000000000000 ) ) ;
#11805 = DIRECTION ( 'NONE',  ( 1.000000000000000000, 0.000000000000000000, 0.000000000000000000 ) ) ;
#11806 = ORIENTED_EDGE ( 'NONE', *, *, #5175, .T. ) ;
#11807 = CARTESIAN_POINT ( 'NONE',  ( 9.968749997951617203, 4.409619785863906571, -2.246813503491833508 ) ) ;
#11808 = FILL_AREA_STYLE ('',( #17911 ) ) ;
#11809 = CARTESIAN_POINT ( 'NONE',  ( 4.861323657744411442, 0.5109457054261445919, -9.843749997951615427 ) ) ;
#11810 = CARTESIAN_POINT ( 'NONE',  ( -22.00000000000000355, 2.694222958124177204E-15, 32.00000000000000000 ) ) ;
#11811 = VERTEX_POINT ( 'NONE', #12041 ) ;
#11812 = CARTESIAN_POINT ( 'NONE',  ( 0.000000000000000000, 0.000000000000000000, -32.00000000000000000 ) ) ;
#11813 = VERTEX_POINT ( 'NONE', #6117 ) ;
#11814 = DIRECTION ( 'NONE',  ( 1.000000000000000000, 0.000000000000000000, 0.000000000000000000 ) ) ;
#11815 = CARTESIAN_POINT ( 'NONE',  ( 6.968749997951614539, 0.7741991708318887166, -4.888101187500000222 ) ) ;
#11816 = DIRECTION ( 'NONE',  ( 1.000000000000000000, 0.000000000000000000, 0.000000000000000000 ) ) ;
#11817 = CARTESIAN_POINT ( 'NONE',  ( -4.762500000000000178, 5.832380380939270108E-16, -6.527800000000000047 ) ) ;
#11818 = AXIS2_PLACEMENT_3D ( 'NONE', #2406, #19117, #11613 ) ;
#11819 = ORIENTED_EDGE ( 'NONE', *, *, #954, .T. ) ;
#11820 = CARTESIAN_POINT ( 'NONE',  ( -3.846120219227966430, -3.114526743279228072, -11.34374999795161543 ) ) ;
#11821 = CARTESIAN_POINT ( 'NONE',  ( -11.00000000000000355, -4.215373648918918192, 3.375000000000000888 ) ) ;
#11822 = ORIENTED_EDGE ( 'NONE', *, *, #12286, .F. ) ;
#11823 = B_SPLINE_CURVE_WITH_KNOTS ( 'NONE', 3,
 ( #19329, #14935, #1226, #2618 ),
 .UNSPECIFIED., .F., .F.,
 ( 4, 4 ),
 ( 2.034713381942770033E-07, 0.0006045424356928436873 ),
 .UNSPECIFIED. ) ;
#11824 = EDGE_CURVE ( 'NONE', #1239, #5054, #12477, .T. ) ;
#11825 = CARTESIAN_POINT ( 'NONE',  ( 12.32184790671639618, 13.12143529358541016, -32.00000000000000000 ) ) ;
#11826 = CARTESIAN_POINT ( 'NONE',  ( -4.611396867937224364, -3.350375938067065906, -15.31249999590322552 ) ) ;
#11827 = VERTEX_POINT ( 'NONE', #18336 ) ;
#11829 = CARTESIAN_POINT ( 'NONE',  ( 0.006974674093433583938, -24.42374957165207405, 2.249040938978413173 ) ) ;
#11828 = VECTOR ( 'NONE', #10199, 1000.000000000000000 ) ;
#11830 = CARTESIAN_POINT ( 'NONE',  ( 10.81249999590322375, 4.840010801796481132, 3.143139765844622957 ) ) ;
#11831 = AXIS2_PLACEMENT_3D ( 'NONE', #7382, #15214, #19305 ) ;
#11832 = FACE_BOUND ( 'NONE', #3564, .T. ) ;
#11833 = ORIENTED_EDGE ( 'NONE', *, *, #7779, .T. ) ;
#11834 = FACE_OUTER_BOUND ( 'NONE', #18037, .T. ) ;
#11835 = ORIENTED_EDGE ( 'NONE', *, *, #5299, .T. ) ;
#11836 = CARTESIAN_POINT ( 'NONE',  ( 0.02436607992775891365, -24.63872515616080960, -2.336989772644527008 ) ) ;
#11837 = ORIENTED_EDGE ( 'NONE', *, *, #10201, .T. ) ;
#11838 = PLANE ( 'NONE',  #19169 ) ;
#11839 = DIRECTION ( 'NONE',  ( -0.000000000000000000, -0.000000000000000000, 1.000000000000000000 ) ) ;
#11840 = CARTESIAN_POINT ( 'NONE',  ( 2.500000000000002220, 1.089935651241147118E-15, 8.800000000000023803 ) ) ;
#11841 = DIRECTION ( 'NONE',  ( -1.000000000000000000, 0.000000000000000000, 0.000000000000000000 ) ) ;
#11842 = CYLINDRICAL_SURFACE ( 'NONE', #14929, 4.200000000000000178 ) ;
#11843 = ORIENTED_EDGE ( 'NONE', *, *, #14921, .T. ) ;
#11844 = EDGE_CURVE ( 'NONE', #11375, #1215, #13635, .T. ) ;
#11845 = AXIS2_PLACEMENT_3D ( 'NONE', #13018, #815, #17612 ) ;
#11846 = AXIS2_PLACEMENT_3D ( 'NONE', #16870, #13862, #12164 ) ;
#11847 = DIRECTION ( 'NONE',  ( 1.000000000000000000, 0.000000000000000000, 0.000000000000000000 ) ) ;
#11848 = ORIENTED_EDGE ( 'NONE', *, *, #13671, .F. ) ;
#11849 = ADVANCED_FACE ( 'NONE', ( #19731 ), #15342, .F. ) ;
#11850 = CARTESIAN_POINT ( 'NONE',  ( -11.00000000000000355, 4.215373648918918192, 3.375000000000000888 ) ) ;
#11851 = DIRECTION ( 'NONE',  ( 0.000000000000000000, 0.000000000000000000, -1.000000000000000000 ) ) ;
#11852 = CYLINDRICAL_SURFACE ( 'NONE', #13933, 1.000000000000002665 ) ;
#11853 = CARTESIAN_POINT ( 'NONE',  ( 12.00000000000000355, 0.000000000000000000, 0.000000000000000000 ) ) ;
#11854 = ORIENTED_EDGE ( 'NONE', *, *, #14531, .T. ) ;
#11855 = CARTESIAN_POINT ( 'NONE',  ( -30.00000000000000000, -6.000000000000000888, 7.347880794884120722E-16 ) ) ;
#11856 = VECTOR ( 'NONE', #13549, 1000.000000000000000 ) ;
#11857 = EDGE_LOOP ( 'NONE', ( #8372, #15640, #8464, #14816 ) ) ;
#11858 = CARTESIAN_POINT ( 'NONE',  ( -4.329756562683109408E-15, -4.945269825389972621E-17, 44.00000000000000711 ) ) ;
#11859 = CARTESIAN_POINT ( 'NONE',  ( -1.988169868018624609, -4.465502636338009701, -9.468749997951615427 ) ) ;
#11860 = DIRECTION ( 'NONE',  ( 0.000000000000000000, 0.000000000000000000, 1.000000000000000000 ) ) ;
#11861 = AXIS2_PLACEMENT_3D ( 'NONE', #7622, #13737, #13638 ) ;
#11862 = VERTEX_POINT ( 'NONE', #1329 ) ;
#11863 = EDGE_LOOP ( 'NONE', ( #7515, #17958, #14662, #7322 ) ) ;
#11864 = FACE_OUTER_BOUND ( 'NONE', #7407, .T. ) ;
#11865 = CARTESIAN_POINT ( 'NONE',  ( 9.468749997951615427, 0.5109457054261445919, 4.861323657744411442 ) ) ;
#11866 = VERTEX_POINT ( 'NONE', #2821 ) ;
#11867 = EDGE_CURVE ( 'NONE', #14187, #13278, #15356, .T. ) ;
#11868 = CARTESIAN_POINT ( 'NONE',  ( 3.814044456245502701, 4.235925505221138643, -10.00000000000000533 ) ) ;
#11869 = EDGE_LOOP ( 'NONE', ( #10716, #3323 ) ) ;
#11870 = CARTESIAN_POINT ( 'NONE',  ( 2.299999999999996270, 0.000000000000000000, 0.000000000000000000 ) ) ;
#11871 = FACE_OUTER_BOUND ( 'NONE', #17973, .T. ) ;
#11872 = ADVANCED_FACE ( 'NONE', ( #7718 ), #5720, .F. ) ;
#11873 = AXIS2_PLACEMENT_3D ( 'NONE', #18713, #617, #14116 ) ;
#11874 = ORIENTED_EDGE ( 'NONE', *, *, #8779, .F. ) ;
#11875 = DIRECTION ( 'NONE',  ( -1.000000000000000000, -0.000000000000000000, -0.000000000000000000 ) ) ;
#11876 = VECTOR ( 'NONE', #810, 1000.000000000000000 ) ;
#11877 = EDGE_CURVE ( 'NONE', #59, #16209, #5560, .T. ) ;
#11878 = CARTESIAN_POINT ( 'NONE',  ( 2.789999999999999147, -18.28042085475289369, 15.74360496233375173 ) ) ;
#11879 = LINE ( 'NONE', #7353, #16429 ) ;
#11880 = FACE_OUTER_BOUND ( 'NONE', #9182, .T. ) ;
#11881 = CARTESIAN_POINT ( 'NONE',  ( 3.476417968967386418, 17.43449690031536292, 35.00000000000000000 ) ) ;
#11882 = FACE_OUTER_BOUND ( 'NONE', #9654, .T. ) ;
#11883 = ORIENTED_EDGE ( 'NONE', *, *, #703, .T. ) ;
#11884 = EDGE_CURVE ( 'NONE', #15571, #6035, #326, .T. ) ;
#11885 = CARTESIAN_POINT ( 'NONE',  ( -19.00000000000000355, -3.434748899119117294, -2.750000000000002220 ) ) ;
#11886 = TOROIDAL_SURFACE ( 'NONE', #77, 24.12539914357697413, 8.000000000000000000 ) ;
#11887 = FACE_BOUND ( 'NONE', #9004, .T. ) ;
#11888 = AXIS2_PLACEMENT_3D ( 'NONE', #4758, #12372, #3362 ) ;
#11889 = CARTESIAN_POINT ( 'NONE',  ( -12.32184790671639085, 13.12143529358541549, -35.00000000000000000 ) ) ;
#11890 = AXIS2_PLACEMENT_3D ( 'NONE', #13126, #3525, #6708 ) ;
#11891 = CARTESIAN_POINT ( 'NONE',  ( 2.790000000000077307, -9.515416771311352662, 22.38018801136472646 ) ) ;
#11892 = CARTESIAN_POINT ( 'NONE',  ( 1.899999999999999023, 0.000000000000000000, 0.000000000000000000 ) ) ;
#11893 = EDGE_CURVE ( 'NONE', #10940, #18392, #7408, .T. ) ;
#11894 = EDGE_LOOP ( 'NONE', ( #6540, #3665, #6754, #13455 ) ) ;
#11895 = ADVANCED_FACE ( 'NONE', ( #18142 ), #4429, .T. ) ;
#11896 = CARTESIAN_POINT ( 'NONE',  ( 2.765633920072239071, -12.59161484032927092, 21.30679549418627161 ) ) ;
#11897 = DIRECTION ( 'NONE',  ( 0.000000000000000000, 0.000000000000000000, 1.000000000000000000 ) ) ;
#11898 = ORIENTED_EDGE ( 'NONE', *, *, #14663, .F. ) ;
#11899 = CARTESIAN_POINT ( 'NONE',  ( 10.81249999590322375, -0.3020334839682879413, 5.763142191869155440 ) ) ;
#11900 = DIRECTION ( 'NONE',  ( 0.000000000000000000, 0.000000000000000000, -1.000000000000000000 ) ) ;
#11901 = AXIS2_PLACEMENT_3D ( 'NONE', #14168, #15478, #6544 ) ;
#11902 =( GEOMETRIC_REPRESENTATION_CONTEXT ( 3 ) GLOBAL_UNCERTAINTY_ASSIGNED_CONTEXT ( ( #19188 ) ) GLOBAL_UNIT_ASSIGNED_CONTEXT ( ( #14367, #12671, #6538 ) ) REPRESENTATION_CONTEXT ( 'NONE', 'WORKASPACE' ) );
#11903 = CARTESIAN_POINT ( 'NONE',  ( 1.039999999999995595, 4.147968289691676524, -27.76164181293047051 ) ) ;
#11904 = CARTESIAN_POINT ( 'NONE',  ( 13.86923836996420789, -11.47363181547641453, 35.00000000000000000 ) ) ;
#11905 = ORIENTED_EDGE ( 'NONE', *, *, #9558, .F. ) ;
#11906 = AXIS2_PLACEMENT_3D ( 'NONE', #2230, #2035, #338 ) ;
#11907 = CARTESIAN_POINT ( 'NONE',  ( 15.19790265903627358, 9.644882309621939598, 32.00000000000000000 ) ) ;
#11908 = CARTESIAN_POINT ( 'NONE',  ( 2.789999999999999147, 9.836394144776026138, -22.71065055754441531 ) ) ;
#11909 = EDGE_CURVE ( 'NONE', #19366, #1940, #17812, .T. ) ;
#11910 = EDGE_CURVE ( 'NONE', #9163, #1573, #16219, .T. ) ;
#11911 = CIRCLE ( 'NONE', #13185, 1.000000000000000888 ) ;
#11912 = FACE_OUTER_BOUND ( 'NONE', #957, .T. ) ;
#11913 = ORIENTED_EDGE ( 'NONE', *, *, #12709, .T. ) ;
#11914 = PLANE ( 'NONE',  #17502 ) ;
#11915 = ORIENTED_EDGE ( 'NONE', *, *, #16085, .T. ) ;
#11916 = DIRECTION ( 'NONE',  ( -1.000000000000000000, 1.224646799147353207E-16, 0.000000000000000000 ) ) ;
#11917 = CARTESIAN_POINT ( 'NONE',  ( 10.34374999795161543, 4.409619785863906571, -2.246813503491833508 ) ) ;
#11918 = DIRECTION ( 'NONE',  ( -1.000000000000000000, -0.000000000000000000, -0.000000000000000000 ) ) ;
#11919 = EDGE_CURVE ( 'NONE', #6321, #1899, #5662, .T. ) ;
#11920 = DIRECTION ( 'NONE',  ( 0.000000000000000000, 0.000000000000000000, -1.000000000000000000 ) ) ;
#11921 = ORIENTED_EDGE ( 'NONE', *, *, #6148, .F. ) ;
#11922 = CARTESIAN_POINT ( 'NONE',  ( -41.99999999999999289, 1.999999999999998224, 5.000000000000000000 ) ) ;
#11923 = ORIENTED_EDGE ( 'NONE', *, *, #4150, .T. ) ;
#11924 = VECTOR ( 'NONE', #18060, 1000.000000000000000 ) ;
#11925 = CIRCLE ( 'NONE', #15126, 0.1999999999999996503 ) ;
#11926 = DIRECTION ( 'NONE',  ( 1.000000000000000000, 0.000000000000000000, 0.000000000000000000 ) ) ;
#11927 = DIRECTION ( 'NONE',  ( 0.000000000000000000, -1.000000000000000000, 0.000000000000000000 ) ) ;
#11928 = EDGE_LOOP ( 'NONE', ( #8424, #15177 ) ) ;
#11929 = CARTESIAN_POINT ( 'NONE',  ( -2.444050593749990341, 4.233219804643887585, -6.468749997951615427 ) ) ;
#11930 = CARTESIAN_POINT ( 'NONE',  ( 8.843749997951615427, 4.861323657744407001, 0.5109457054261780096 ) ) ;
#11931 = DIRECTION ( 'NONE',  ( 0.000000000000000000, 0.000000000000000000, -1.000000000000000000 ) ) ;
#11932 = EDGE_CURVE ( 'NONE', #3033, #6213, #11227, .T. ) ;
#11933 = ORIENTED_EDGE ( 'NONE', *, *, #5890, .F. ) ;
#11934 = LINE ( 'NONE', #1431, #18863 ) ;
#11935 = ORIENTED_EDGE ( 'NONE', *, *, #5520, .F. ) ;
#11936 = CARTESIAN_POINT ( 'NONE',  ( 2.601776121706763423, 19.18368891937490517, 17.47009390565497711 ) ) ;
#11937 = ORIENTED_EDGE ( 'NONE', *, *, #13174, .T. ) ;
#11938 =( NAMED_UNIT ( * ) SI_UNIT ( $, .STERADIAN. ) SOLID_ANGLE_UNIT ( ) );
#11939 = CIRCLE ( 'NONE', #1402, 4.400000000000000355 ) ;
#11940 = CARTESIAN_POINT ( 'NONE',  ( -8.671566133830875600, 15.77352024078954429, 32.00000000000000000 ) ) ;
#11941 = CARTESIAN_POINT ( 'NONE',  ( 3.954556930911842016, -2.873153789725853002, -8.468749997951615427 ) ) ;
#11942 = CARTESIAN_POINT ( 'NONE',  ( 12.46874999795161543, -1.016293382781378485, -4.781284448697201483 ) ) ;
#11943 = CARTESIAN_POINT ( 'NONE',  ( 13.00000000000000178, 0.5236311934647676081, 4.860400829920955346 ) ) ;
#11944 = EDGE_CURVE ( 'NONE', #6719, #9660, #16069, .T. ) ;
#11945 = ORIENTED_EDGE ( 'NONE', *, *, #6979, .T. ) ;
#11946 = CARTESIAN_POINT ( 'NONE',  ( 2.031033479673587827, -19.12621924769852555, -19.86422722021333342 ) ) ;
#11947 = MECHANICAL_DESIGN_GEOMETRIC_PRESENTATION_REPRESENTATION (  '', ( #11327 ), #11629 ) ;
#11948 = CARTESIAN_POINT ( 'NONE',  ( 2.601776105308176046, -2.857713464478872201, 25.78859396478526733 ) ) ;
#11949 = PRODUCT_DEFINITION_SHAPE ( 'NONE', 'NONE',  #8823 ) ;
#11950 = VERTEX_POINT ( 'NONE', #9438 ) ;
#11951 = EDGE_CURVE ( 'NONE', #2783, #17931, #9852, .T. ) ;
#11952 = CLOSED_SHELL ( 'NONE', ( #15535, #16769, #1241, #2873, #16855, #9834 ) ) ;
#11953 = CARTESIAN_POINT ( 'NONE',  ( 10.00000000000000533, 5.421022142882375938, -1.761396867937200739 ) ) ;
#11954 = LINE ( 'NONE', #16560, #14152 ) ;
#11955 = DIRECTION ( 'NONE',  ( 0.000000000000000000, 0.000000000000000000, -1.000000000000000000 ) ) ;
#11956 = FACE_OUTER_BOUND ( 'NONE', #18903, .T. ) ;
#11957 = DIRECTION ( 'NONE',  ( 0.000000000000000000, 0.000000000000000000, 1.000000000000000000 ) ) ;
#11958 = ORIENTED_EDGE ( 'NONE', *, *, #19165, .F. ) ;
#11959 = LINE ( 'NONE', #2743, #19625 ) ;
#11960 = CIRCLE ( 'NONE', #3336, 1.000000000000004441 ) ;
#11961 =( NAMED_UNIT ( * ) SI_UNIT ( $, .STERADIAN. ) SOLID_ANGLE_UNIT ( ) );
#11962 = CARTESIAN_POINT ( 'NONE',  ( -4.780397808154247308, 1.280903732194486722, -13.96874999795161365 ) ) ;
#11963 = CARTESIAN_POINT ( 'NONE',  ( 2.068159791354145849, -5.387740456496247887, -7.812499995903224637 ) ) ;
#11964 = VERTEX_POINT ( 'NONE', #2118 ) ;
#11965 = ORIENTED_EDGE ( 'NONE', *, *, #14059, .F. ) ;
#11966 = PLANE ( 'NONE',  #8901 ) ;
#11967 = B_SPLINE_CURVE_WITH_KNOTS ( 'NONE', 3,
 ( #931, #16148, #13324, #1021, #19040, #7298 ),
 .UNSPECIFIED., .F., .F.,
 ( 4, 2, 4 ),
 ( 2.380731676442874196E-07, 0.002318718087522266338, 0.004637198101876887496 ),
 .UNSPECIFIED. ) ;
#11968 = CYLINDRICAL_SURFACE ( 'NONE', #16533, 8.073750000000021743 ) ;
#11969 = EDGE_CURVE ( 'NONE', #540, #17188, #18827, .T. ) ;
#11971 = ORIENTED_EDGE ( 'NONE', *, *, #453, .F. ) ;
#11970 = CIRCLE ( 'NONE', #8135, 28.06981291497571007 ) ;
#11972 = DIRECTION ( 'NONE',  ( 0.9135454576425977580, -0.4067366430758074247, 0.000000000000000000 ) ) ;
#11973 = ORIENTED_EDGE ( 'NONE', *, *, #19384, .F. ) ;
#11974 = CARTESIAN_POINT ( 'NONE',  ( -22.50000000000000711, 0.000000000000000000, 0.000000000000000000 ) ) ;
#11975 = LINE ( 'NONE', #2758, #3233 ) ;
#11976 = B_SPLINE_CURVE_WITH_KNOTS ( 'NONE', 3,
 ( #3974, #12784, #5367, #19268, #9795, #18980 ),
 .UNSPECIFIED., .F., .F.,
 ( 4, 2, 4 ),
 ( 4.462636695653741059E-07, 0.001879885036799761782, 0.003759323809929957915 ),
 .UNSPECIFIED. ) ;
#11977 = ORIENTED_EDGE ( 'NONE', *, *, #1500, .T. ) ;
#11978 = FACE_OUTER_BOUND ( 'NONE', #9587, .T. ) ;
#11979 = CARTESIAN_POINT ( 'NONE',  ( 13.31249999590322730, 5.421022142882376826, 1.761396867937200073 ) ) ;
#11980 = EDGE_CURVE ( 'NONE', #3279, #123, #9334, .T. ) ;
#11981 = EDGE_CURVE ( 'NONE', #3813, #7592, #8552, .T. ) ;
#11982 = DIRECTION ( 'NONE',  ( 0.000000000000000000, 0.000000000000000000, -1.000000000000000000 ) ) ;
#11983 = ORIENTED_EDGE ( 'NONE', *, *, #12944, .T. ) ;
#11984 = CARTESIAN_POINT ( 'NONE',  ( 1.394999999999999574, 27.68468304288259318, 4.633866840649019103 ) ) ;
#11985 = CYLINDRICAL_SURFACE ( 'NONE', #3262, 1.000000000000004441 ) ;
#11986 = ORIENTED_EDGE ( 'NONE', *, *, #7969, .T. ) ;
#11987 = DIRECTION ( 'NONE',  ( 1.000000000000000000, 0.000000000000000000, 0.000000000000000000 ) ) ;
#11988 = AXIS2_PLACEMENT_3D ( 'NONE', #11291, #11484, #11580 ) ;
#11989 = DIRECTION ( 'NONE',  ( -1.000000000000000000, 0.000000000000000000, -0.000000000000000000 ) ) ;
#11990 = UNCERTAINTY_MEASURE_WITH_UNIT (LENGTH_MEASURE( 1.000000000000000082E-05 ), #18020, 'distance_accuracy_value', 'NONE');
#11991 = VECTOR ( 'NONE', #14647, 1000.000000000000000 ) ;
#11992 = DIRECTION ( 'NONE',  ( -0.000000000000000000, -0.000000000000000000, 1.000000000000000000 ) ) ;
#11993 = EDGE_CURVE ( 'NONE', #17321, #14722, #2790, .T. ) ;
#11994 = FACE_OUTER_BOUND ( 'NONE', #9212, .T. ) ;
#11995 = CARTESIAN_POINT ( 'NONE',  ( 89.62500000000000000, 0.000000000000000000, 0.000000000000000000 ) ) ;
#11996 = ORIENTED_EDGE ( 'NONE', *, *, #3718, .F. ) ;
#11997 = CYLINDRICAL_SURFACE ( 'NONE', #10920, 8.000000000000000000 ) ;
#11998 = CARTESIAN_POINT ( 'NONE',  ( 10.64522241986047568, 2.725425358843983450E-16, 5.700000000000002842 ) ) ;
#11999 = VERTEX_POINT ( 'NONE', #227 ) ;
#12000 = B_SPLINE_CURVE_WITH_KNOTS ( 'NONE', 3,
 ( #9506, #7985, #15508, #3493 ),
 .UNSPECIFIED., .F., .F.,
 ( 4, 4 ),
 ( 4.462636695580848051E-07, 0.0004963285629697519611 ),
 .UNSPECIFIED. ) ;
#12001 = CARTESIAN_POINT ( 'NONE',  ( 9.812499995903223748, -5.574407415329147852, -1.493657965219562511 ) ) ;
#12002 = AXIS2_PLACEMENT_3D ( 'NONE', #18437, #7624, #4730 ) ;
#12003 = B_SPLINE_CURVE_WITH_KNOTS ( 'NONE', 3,
 ( #5792, #8911, #2599, #2696, #16418, #15014 ),
 .UNSPECIFIED., .F., .F.,
 ( 4, 2, 4 ),
 ( 2.032124546190077199E-07, 0.001878594002992309232, 0.003756984793529999193 ),
 .UNSPECIFIED. ) ;
#12004 = CIRCLE ( 'NONE', #3058, 4.000000000000000000 ) ;
#12005 = CARTESIAN_POINT ( 'NONE',  ( 0.02436607992776455150, 21.30679549418631780, 12.59161484032919986 ) ) ;
#12006 = LINE ( 'NONE', #4201, #18647 ) ;
#12007 = ORIENTED_EDGE ( 'NONE', *, *, #14616, .T. ) ;
#12008 = DIRECTION ( 'NONE',  ( 1.000000000000000000, 0.000000000000000000, 0.000000000000000000 ) ) ;
#12009 = SURFACE_STYLE_FILL_AREA ( #15010 ) ;
#12010 = DIRECTION ( 'NONE',  ( 1.000000000000000000, 0.000000000000000000, 0.000000000000000000 ) ) ;
#12011 =( NAMED_UNIT ( * ) PLANE_ANGLE_UNIT ( ) SI_UNIT ( $, .RADIAN. ) );
#12012 = EDGE_LOOP ( 'NONE', ( #9637, #16152, #17733, #6195 ) ) ;
#12013 = DIRECTION ( 'NONE',  ( -0.000000000000000000, -0.000000000000000000, 1.000000000000000000 ) ) ;
#12014 = ORIENTED_EDGE ( 'NONE', *, *, #1520, .T. ) ;
#12015 = CARTESIAN_POINT ( 'NONE',  ( 4.611396867937200383, 3.350375938067097881, -15.31249999590322552 ) ) ;
#12016 = EDGE_CURVE ( 'NONE', #1514, #12259, #6796, .T. ) ;
#12017 = CARTESIAN_POINT ( 'NONE',  ( 6.626241948324199882, -16.73597674598852691, 32.00000000000000000 ) ) ;
#12018 =( BOUNDED_CURVE ( )  B_SPLINE_CURVE ( 2, ( #5528, #17739, #10144, #7111, #13242, #11734, #4722, #5915, #7714, #1620, #18044, #1324, #16540, #12233, #1528 ),
 .UNSPECIFIED., .F., .F. ) 
 B_SPLINE_CURVE_WITH_KNOTS ( ( 3, 2, 2, 2, 2, 2, 2, 3 ),
 ( 0.000000000000000000, 0.05000000000000000971, 0.1000000000000000194, 0.1499999999999999944, 0.2000000000000000389, 0.2500000000000000000, 0.2999999999999999889, 0.3265529187307102399 ),
 .UNSPECIFIED. ) 
 CURVE ( )  GEOMETRIC_REPRESENTATION_ITEM ( )  RATIONAL_B_SPLINE_CURVE ( ( 1.000000000000000000, 0.9876883405951377704, 1.000000000000000000, 0.9876883405951377704, 1.000000000000000000, 0.9876883405951377704, 1.000000000000000000, 0.9876883405951377704, 1.000000000000000000, 0.9876883405951377704, 1.000000000000000000, 0.9876883405951377704, 1.000000000000000000, 0.9934617901676501273, 0.9938679225082089896 ) ) 
 REPRESENTATION_ITEM ( '' )  );
#12019 = EDGE_CURVE ( 'NONE', #2597, #1514, #11030, .T. ) ;
#12020 = LINE ( 'NONE', #7093, #11562 ) ;
#12021 = CIRCLE ( 'NONE', #4672, 14.00000000000000178 ) ;
#12022 = CARTESIAN_POINT ( 'NONE',  ( 4.781284448697195266, 1.016293382781411792, -12.84374999795161543 ) ) ;
#12023 = CIRCLE ( 'NONE', #15226, 28.06981291497571362 ) ;
#12024 = ORIENTED_EDGE ( 'NONE', *, *, #7953, .F. ) ;
#12025 = DIRECTION ( 'NONE',  ( 1.000000000000000000, 0.000000000000000000, 0.000000000000000000 ) ) ;
#12026 = DIRECTION ( 'NONE',  ( -1.000000000000000000, -0.000000000000000000, -0.000000000000000000 ) ) ;
#12027 = VERTEX_POINT ( 'NONE', #18530 ) ;
#12028 = ADVANCED_FACE ( 'NONE', ( #4927 ), #6603, .F. ) ;
#12029 = CARTESIAN_POINT ( 'NONE',  ( 2.873153789725825025, 3.954556930911862000, -13.46874999795161543 ) ) ;
#12030 = CARTESIAN_POINT ( 'NONE',  ( 4.888101187500000222, -3.413342815706642518E-14, -6.843749997951615427 ) ) ;
#12031 = ORIENTED_EDGE ( 'NONE', *, *, #4043, .F. ) ;
#12032 = CIRCLE ( 'NONE', #3407, 4.000000000000000000 ) ;
#12033 = CARTESIAN_POINT ( 'NONE',  ( 2.695436003842732298, 4.150607464521791634, -10.34374999795161543 ) ) ;
#12034 = DIRECTION ( 'NONE',  ( 0.000000000000000000, 0.000000000000000000, -1.000000000000000000 ) ) ;
#12035 = EDGE_CURVE ( 'NONE', #19497, #6719, #6756, .T. ) ;
#12036 = CARTESIAN_POINT ( 'NONE',  ( -25.31088913245540084, -1.027644533213482535E-13, 37.99999999999999289 ) ) ;
#12037 = AXIS2_PLACEMENT_3D ( 'NONE', #7270, #13392, #18100 ) ;
#12038 = ORIENTED_EDGE ( 'NONE', *, *, #15449, .F. ) ;
#12039 = CARTESIAN_POINT ( 'NONE',  ( 2.000000000000001776, 1.012170579495290078E-15, 8.265000000000021885 ) ) ;
#12040 = ORIENTED_EDGE ( 'NONE', *, *, #15945, .F. ) ;
#12041 = CARTESIAN_POINT ( 'NONE',  ( -18.11901729331277267, 5.562305898749051458, -32.00000000000000000 ) ) ;
#12042 = ORIENTED_EDGE ( 'NONE', *, *, #18823, .F. ) ;
#12043 = CARTESIAN_POINT ( 'NONE',  ( 2.789999999999999147, 1.991882183130632589, -24.04302995059963877 ) ) ;
#12044 = LINE ( 'NONE', #1436, #15708 ) ;
#12045 = LINE ( 'NONE', #16849, #10192 ) ;
#12046 = CARTESIAN_POINT ( 'NONE',  ( 9.000000000000005329, -5.207209108562803834, -2.318398865532109721 ) ) ;
#12047 = CARTESIAN_POINT ( 'NONE',  ( 13.00000000000000178, 0.5876048313370836329, 4.852654302691283839 ) ) ;
#12048 = VERTEX_POINT ( 'NONE', #424 ) ;
#12049 = CARTESIAN_POINT ( 'NONE',  ( 2.255998204157473097, -17.85806462366060288, -32.00000000000000000 ) ) ;
#12050 = AXIS2_PLACEMENT_3D ( 'NONE', #17080, #12284, #1868 ) ;
#12051 = VECTOR ( 'NONE', #4804, 1000.000000000000000 ) ;
#12052 = CARTESIAN_POINT ( 'NONE',  ( 13.00000000000000178, 0.000000000000000000, 0.000000000000000000 ) ) ;
#12053 = EDGE_CURVE ( 'NONE', #15383, #3340, #14623, .T. ) ;
#12054 = VERTEX_POINT ( 'NONE', #8521 ) ;
#12055 = CARTESIAN_POINT ( 'NONE',  ( 13.00000000000000178, 3.789407127742559833, -3.087705756618140285 ) ) ;
#12056 = CARTESIAN_POINT ( 'NONE',  ( -5.209999999999999964, 0.000000000000000000, 0.000000000000000000 ) ) ;
#12057 = ORIENTED_EDGE ( 'NONE', *, *, #14193, .T. ) ;
#12058 = FACE_OUTER_BOUND ( 'NONE', #3421, .T. ) ;
#12059 = CARTESIAN_POINT ( 'NONE',  ( 11.06250000000000000, 0.000000000000000000, 0.000000000000000000 ) ) ;
#12060 = DIRECTION ( 'NONE',  ( 0.000000000000000000, 0.000000000000000000, 1.000000000000000000 ) ) ;
#12061 = ORIENTED_EDGE ( 'NONE', *, *, #15186, .T. ) ;
#12062 = CARTESIAN_POINT ( 'NONE',  ( 12.46874999795161543, -1.016293382781378485, -4.781284448697201483 ) ) ;
#12063 = AXIS2_PLACEMENT_3D ( 'NONE', #10418, #2895, #15116 ) ;
#12064 = ORIENTED_EDGE ( 'NONE', *, *, #17036, .T. ) ;
#12065 = DIRECTION ( 'NONE',  ( 1.000000000000000000, 0.000000000000000000, 0.000000000000000000 ) ) ;
#12066 = CARTESIAN_POINT ( 'NONE',  ( 1.394999999999999574, -24.89775460606823287, -12.96210679857813908 ) ) ;
#12067 = AXIS2_PLACEMENT_3D ( 'NONE', #7217, #1238, #8463 ) ;
#12068 = CARTESIAN_POINT ( 'NONE',  ( 2.999999999999998224, 0.000000000000000000, 0.000000000000000000 ) ) ;
#12069 = ORIENTED_EDGE ( 'NONE', *, *, #1341, .F. ) ;
#12070 = VERTEX_POINT ( 'NONE', #14329 ) ;
#12071 = DIRECTION ( 'NONE',  ( 1.000000000000000000, 0.000000000000000000, 0.000000000000000000 ) ) ;
#12072 = CARTESIAN_POINT ( 'NONE',  ( 1.493657965219523875, 5.574407415329156734, -9.812499995903223748 ) ) ;
#12073 = ORIENTED_EDGE ( 'NONE', *, *, #11368, .T. ) ;
#12074 = CARTESIAN_POINT ( 'NONE',  ( 0.07186815222488067423, -24.78765742476142719, 5.344160105508607650 ) ) ;
#12075 = ORIENTED_EDGE ( 'NONE', *, *, #3034, .F. ) ;
#12076 = LINE ( 'NONE', #7653, #1036 ) ;
#12077 = SHAPE_REPRESENTATION ( 'brake cone', ( #16724 ), #3651 ) ;
#12078 = EDGE_CURVE ( 'NONE', #6035, #4236, #14630, .T. ) ;
#12079 = VECTOR ( 'NONE', #19584, 1000.000000000000000 ) ;
#12080 = ORIENTED_EDGE ( 'NONE', *, *, #1128, .T. ) ;
#12081 = AXIS2_PLACEMENT_3D ( 'NONE', #17825, #8437, #19315 ) ;
#12082 = EDGE_CURVE ( 'NONE', #9272, #5021, #10222, .T. ) ;
#12083 = CARTESIAN_POINT ( 'NONE',  ( -1.310841663519413114, 0.000000000000000000, 0.000000000000000000 ) ) ;
#12084 = LINE ( 'NONE', #10486, #16762 ) ;
#12085 = CARTESIAN_POINT ( 'NONE',  ( 0.02436607992775717893, -9.836394144775869819, 22.71065055754449347 ) ) ;
#12086 = ORIENTED_EDGE ( 'NONE', *, *, #14578, .F. ) ;
#12087 = CARTESIAN_POINT ( 'NONE',  ( 1.749999999999998002, 0.000000000000000000, 0.000000000000000000 ) ) ;
#12088 = FACE_BOUND ( 'NONE', #17314, .T. ) ;
#12089 = ORIENTED_EDGE ( 'NONE', *, *, #503, .F. ) ;
#12090 = DIRECTION ( 'NONE',  ( 1.000000000000000000, 0.000000000000000000, 0.000000000000000000 ) ) ;
#12091 = CIRCLE ( 'NONE', #2820, 5.700000000000001954 ) ;
#12092 = PLANE ( 'NONE',  #6599 ) ;
#12093 = DIRECTION ( 'NONE',  ( 1.000000000000000000, 0.000000000000000000, 0.000000000000000000 ) ) ;
#12094 = CIRCLE ( 'NONE', #16565, 6.000000000000000888 ) ;
#12095 = DIRECTION ( 'NONE',  ( 1.000000000000000000, 0.000000000000000000, 0.000000000000000000 ) ) ;
#12096 = FACE_OUTER_BOUND ( 'NONE', #8886, .T. ) ;
#12097 = VERTEX_POINT ( 'NONE', #827 ) ;
#12098 = DIRECTION ( 'NONE',  ( -1.000000000000000000, 0.000000000000000000, 0.000000000000000000 ) ) ;
#12099 = EDGE_CURVE ( 'NONE', #9666, #1561, #18130, .T. ) ;
#12100 = CARTESIAN_POINT ( 'NONE',  ( -1.280903732194386802, 4.780397808154273065, -13.96874999795161365 ) ) ;
#12101 = VERTEX_POINT ( 'NONE', #5411 ) ;
#12102 = CARTESIAN_POINT ( 'NONE',  ( 6.968749997951614539, -3.846120219227901149, -3.114526743279308896 ) ) ;
#12103 = DIRECTION ( 'NONE',  ( 0.000000000000000000, 0.000000000000000000, 1.000000000000000000 ) ) ;
#12104 = CIRCLE ( 'NONE', #4116, 1.000000000000002665 ) ;
#12105 = ADVANCED_FACE ( 'NONE', ( #6703 ), #12827, .F. ) ;
#12106 = DIRECTION ( 'NONE',  ( -0.000000000000000000, -0.000000000000000000, 1.000000000000000000 ) ) ;
#12107 = DIRECTION ( 'NONE',  ( -1.000000000000000000, -0.000000000000000000, 0.000000000000000000 ) ) ;
#12108 = ORIENTED_EDGE ( 'NONE', *, *, #1468, .F. ) ;
#12109 = CYLINDRICAL_SURFACE ( 'NONE', #859, 5.700000000000001954 ) ;
#12110 = DIRECTION ( 'NONE',  ( -0.000000000000000000, -0.000000000000000000, 1.000000000000000000 ) ) ;
#12111 = AXIS2_PLACEMENT_3D ( 'NONE', #2646, #18067, #17865 ) ;
#12112 = CARTESIAN_POINT ( 'NONE',  ( 12.00000000000000533, -5.421022142882365280, -1.761396867937238042 ) ) ;
#12113 = ORIENTED_EDGE ( 'NONE', *, *, #8123, .F. ) ;
#12114 = FACE_OUTER_BOUND ( 'NONE', #19417, .T. ) ;
#12115 = DIRECTION ( 'NONE',  ( 0.000000000000000000, -0.6818181818181822118, 0.7315216790650489465 ) ) ;
#12116 = CARTESIAN_POINT ( 'NONE',  ( 17.96448111170888851, 1.130229351527639148, -35.00000000000000000 ) ) ;
#12117 = DIRECTION ( 'NONE',  ( 1.000000000000000000, 0.000000000000000000, 0.000000000000000000 ) ) ;
#12118 = DIRECTION ( 'NONE',  ( -1.000000000000000000, 0.000000000000000000, 0.000000000000000000 ) ) ;
#12119 = AXIS2_PLACEMENT_3D ( 'NONE', #11162, #14361, #3548 ) ;
#12120 = B_SPLINE_CURVE_WITH_KNOTS ( 'NONE', 3,
 ( #13084, #19178, #5471, #975, #3681, #16097 ),
 .UNSPECIFIED., .F., .F.,
 ( 4, 2, 4 ),
 ( 2.586195665736120714E-07, 0.001878649493629690539, 0.003757040367692807744 ),
 .UNSPECIFIED. ) ;
#12121 = CARTESIAN_POINT ( 'NONE',  ( 4.476417968967386862, 17.43449690031536292, -32.00000000000000000 ) ) ;
#12122 = ORIENTED_EDGE ( 'NONE', *, *, #2356, .F. ) ;
#12123 = CARTESIAN_POINT ( 'NONE',  ( -4.465502636338010589, 1.988169868018623720, -14.46874999795161720 ) ) ;
#12124 = EDGE_CURVE ( 'NONE', #7035, #8351, #6298, .T. ) ;
#12125 = DIRECTION ( 'NONE',  ( 0.000000000000000000, 0.000000000000000000, 1.000000000000000000 ) ) ;
#12126 = ORIENTED_EDGE ( 'NONE', *, *, #5090, .T. ) ;
#12127 = EDGE_CURVE ( 'NONE', #19487, #1162, #19721, .T. ) ;
#12128 = CARTESIAN_POINT ( 'NONE',  ( -1.510506337161861667, 4.648860486681953397, -10.84374999795161543 ) ) ;
#12129 = FACE_OUTER_BOUND ( 'NONE', #1823, .T. ) ;
#12130 = EDGE_CURVE ( 'NONE', #13685, #8919, #15931, .T. ) ;
#12131 = VERTEX_POINT ( 'NONE', #16026 ) ;
#12132 = APPLICATION_CONTEXT ( 'automotive_design' ) ;
#12133 = FACE_OUTER_BOUND ( 'NONE', #17240, .T. ) ;
#12134 = CARTESIAN_POINT ( 'NONE',  ( 9.843749997951615427, 4.465502636338024800, 1.988169868018593300 ) ) ;
#12135 = CARTESIAN_POINT ( 'NONE',  ( 5.476417968967387750, 17.43449690031536292, 32.00000000000000000 ) ) ;
#12136 = ORIENTED_EDGE ( 'NONE', *, *, #17837, .F. ) ;
#12137 = DIRECTION ( 'NONE',  ( 1.000000000000000000, 0.000000000000000000, 0.000000000000000000 ) ) ;
#12138 = ORIENTED_EDGE ( 'NONE', *, *, #2486, .F. ) ;
#12139 = CARTESIAN_POINT ( 'NONE',  ( -7.937500000000000000, -4.582717761692664205, -0.7089489049740167470 ) ) ;
#12140 = EDGE_LOOP ( 'NONE', ( #17665, #12814, #11061, #11129 ) ) ;
#12141 = AXIS2_PLACEMENT_3D ( 'NONE', #2046, #8151, #10859 ) ;
#12142 = SURFACE_STYLE_USAGE ( .BOTH. , #4336 ) ;
#12143 = CARTESIAN_POINT ( 'NONE',  ( 1.960886852992497653, -24.44424927289185590, 12.96989951879399072 ) ) ;
#12144 = EDGE_CURVE ( 'NONE', #9713, #13429, #2238, .T. ) ;
#12145 = DIRECTION ( 'NONE',  ( 1.000000000000000000, 0.000000000000000000, 0.000000000000000000 ) ) ;
#12146 = DIRECTION ( 'NONE',  ( 1.000000000000000000, 0.000000000000000000, 0.000000000000000000 ) ) ;
#12147 = CARTESIAN_POINT ( 'NONE',  ( -15.00000000000000355, -3.434748899119118182, -2.750000000000002665 ) ) ;
#12148 = ORIENTED_EDGE ( 'NONE', *, *, #3954, .T. ) ;
#12149 = CARTESIAN_POINT ( 'NONE',  ( 18.68117051311639543, -3.372863662543048591, -32.00000000000000000 ) ) ;
#12150 = EDGE_CURVE ( 'NONE', #19072, #253, #1029, .T. ) ;
#12151 = CIRCLE ( 'NONE', #16617, 0.9999999999999974465 ) ;
#12152 = ORIENTED_EDGE ( 'NONE', *, *, #2731, .T. ) ;
#12153 = AXIS2_PLACEMENT_3D ( 'NONE', #5718, #16339, #19635 ) ;
#12154 = FACE_OUTER_BOUND ( 'NONE', #6381, .T. ) ;
#12155 = DIRECTION ( 'NONE',  ( -1.000000000000000000, -0.000000000000000000, -0.000000000000000000 ) ) ;
#12156 = ORIENTED_EDGE ( 'NONE', *, *, #6435, .T. ) ;
#12157 = FACE_OUTER_BOUND ( 'NONE', #7139, .T. ) ;
#12158 = CARTESIAN_POINT ( 'NONE',  ( -3.000000000000002665, 0.000000000000000000, 10.00000000000000000 ) ) ;
#12159 = DIRECTION ( 'NONE',  ( 1.000000000000000000, 1.224646799147353207E-16, 0.000000000000000000 ) ) ;
#12160 = ORIENTED_EDGE ( 'NONE', *, *, #10260, .T. ) ;
#12161 = CARTESIAN_POINT ( 'NONE',  ( 13.00000000000000000, -0.2080849974988778772, -4.883670121236158401 ) ) ;
#12162 = DIRECTION ( 'NONE',  ( 0.000000000000000000, 0.000000000000000000, 1.000000000000000000 ) ) ;
#12163 = CARTESIAN_POINT ( 'NONE',  ( -15.19790265903627180, 9.644882309621941374, 32.00000000000000000 ) ) ;
#12164 = DIRECTION ( 'NONE',  ( 0.000000000000000000, 0.000000000000000000, 1.000000000000000000 ) ) ;
#12165 = EDGE_CURVE ( 'NONE', #11862, #6062, #15266, .T. ) ;
#12166 = ORIENTED_EDGE ( 'NONE', *, *, #2684, .F. ) ;
#12167 = EDGE_LOOP ( 'NONE', ( #13596, #15165 ) ) ;
#12168 = CARTESIAN_POINT ( 'NONE',  ( 0.7592463834391185440, 12.05220173035438513, 24.80264696524887214 ) ) ;
#12169 = AXIS2_PLACEMENT_3D ( 'NONE', #9491, #1683, #16895 ) ;
#12170 = CARTESIAN_POINT ( 'NONE',  ( 10.84374999795161543, 4.648860486681953397, -1.510506337161861667 ) ) ;
#12171 = ORIENTED_EDGE ( 'NONE', *, *, #10817, .T. ) ;
#12172 = DIRECTION ( 'NONE',  ( 1.000000000000000000, 0.000000000000000000, 0.000000000000000000 ) ) ;
#12173 = VERTEX_POINT ( 'NONE', #3817 ) ;
#12174 = CARTESIAN_POINT ( 'NONE',  ( 0.5109457054261454800, -4.861323657744410554, -14.46874999795161720 ) ) ;
#12175 = ORIENTED_EDGE ( 'NONE', *, *, #11981, .F. ) ;
#12176 = FACE_OUTER_BOUND ( 'NONE', #3509, .T. ) ;
#12177 = CARTESIAN_POINT ( 'NONE',  ( 11.81249999590322552, 5.699999999999999289, -0.9027913098498572264 ) ) ;
#12178 = CARTESIAN_POINT ( 'NONE',  ( 10.58013454126452046, -14.56230589874905412, -35.00000000000000000 ) ) ;
#12179 = ORIENTED_EDGE ( 'NONE', *, *, #13258, .F. ) ;
#12180 = CARTESIAN_POINT ( 'NONE',  ( 9.000000000000001776, 0.000000000000000000, 0.000000000000000000 ) ) ;
#12181 = CARTESIAN_POINT ( 'NONE',  ( -11.00000000000000355, -4.200000000000001066, 0.000000000000000000 ) ) ;
#12182 = EDGE_CURVE ( 'NONE', #16673, #11527, #1847, .T. ) ;
#12183 = ORIENTED_EDGE ( 'NONE', *, *, #18006, .T. ) ;
#12184 = FACE_OUTER_BOUND ( 'NONE', #19775, .T. ) ;
#12185 = CARTESIAN_POINT ( 'NONE',  ( 0.000000000000000000, 0.000000000000000000, 0.000000000000000000 ) ) ;
#12186 = CARTESIAN_POINT ( 'NONE',  ( 0.1882238946918228795, -25.78859396478530641, 2.857713464478602194 ) ) ;
#12187 = CARTESIAN_POINT ( 'NONE',  ( -15.00000000000000355, 0.000000000000000000, 0.000000000000000000 ) ) ;
#12188 = AXIS2_PLACEMENT_3D ( 'NONE', #6416, #5036, #9652 ) ;
#12189 = CARTESIAN_POINT ( 'NONE',  ( 1.510506337161861223, 4.648860486681953397, -12.84374999795161543 ) ) ;
#12190 = AXIS2_PLACEMENT_3D ( 'NONE', #14239, #8020, #9244 ) ;
#12191 = EDGE_CURVE ( 'NONE', #11206, #16982, #7904, .T. ) ;
#12192 = VERTEX_POINT ( 'NONE', #8319 ) ;
#12193 = DIRECTION ( 'NONE',  ( -1.000000000000000000, -0.000000000000000000, -0.000000000000000000 ) ) ;
#12194 = AXIS2_PLACEMENT_3D ( 'NONE', #7313, #14942, #4525 ) ;
#12195 = CYLINDRICAL_SURFACE ( 'NONE', #18738, 9.000000000000001776 ) ;
#12196 = EDGE_LOOP ( 'NONE', ( #11627, #13437 ) ) ;
#12197 = CARTESIAN_POINT ( 'NONE',  ( 6.000000000000005329, -4.936344801571327601, 2.849999999999954348 ) ) ;
#12198 = CARTESIAN_POINT ( 'NONE',  ( -5.574407415329146964, 1.493657965219562067, -14.81249999590322375 ) ) ;
#12199 = EDGE_CURVE ( 'NONE', #677, #8962, #12927, .T. ) ;
#12200 = CARTESIAN_POINT ( 'NONE',  ( 0.07186813532171051899, 2.577209017047360717, -25.22589920183358814 ) ) ;
#12201 = CARTESIAN_POINT ( 'NONE',  ( -3.968750000000007994, -6.874076642538976323, 0.000000000000000000 ) ) ;
#12202 = ORIENTED_EDGE ( 'NONE', *, *, #16901, .T. ) ;
#12203 = AXIS2_PLACEMENT_3D ( 'NONE', #17734, #4027, #5331 ) ;
#12204 = AXIS2_PLACEMENT_3D ( 'NONE', #6361, #7781, #9395 ) ;
#12205 = CARTESIAN_POINT ( 'NONE',  ( 2.765633920072238183, 2.336989772644269436, 24.63872515616083447 ) ) ;
#12206 = FILL_AREA_STYLE ('',( #16714 ) ) ;
#12207 = CARTESIAN_POINT ( 'NONE',  ( 0.5109457054261454800, -4.861323657744410554, -14.84374999795161543 ) ) ;
#12208 = CIRCLE ( 'NONE', #3574, 24.12539914357697768 ) ;
#12209 = DIRECTION ( 'NONE',  ( 0.9773501006361904331, 0.000000000000000000, -0.2116288751244229938 ) ) ;
#12210 = ORIENTED_EDGE ( 'NONE', *, *, #9972, .F. ) ;
#12211 = DIRECTION ( 'NONE',  ( 0.000000000000000000, -0.9510565162951523099, -0.3090169943749515591 ) ) ;
#12212 = CARTESIAN_POINT ( 'NONE',  ( 2.765633920072242624, 9.836394144775706394, 22.71065055754456097 ) ) ;
#12213 = CARTESIAN_POINT ( 'NONE',  ( 2.789999999999999147, 0.000000000000000000, 0.000000000000000000 ) ) ;
#12214 =( GEOMETRIC_REPRESENTATION_CONTEXT ( 3 ) GLOBAL_UNCERTAINTY_ASSIGNED_CONTEXT ( ( #10224 ) ) GLOBAL_UNIT_ASSIGNED_CONTEXT ( ( #13882, #363, #5064 ) ) REPRESENTATION_CONTEXT ( 'NONE', 'WORKASPACE' ) );
#12215 = CARTESIAN_POINT ( 'NONE',  ( -2.299999999999996270, 0.000000000000000000, 0.000000000000000000 ) ) ;
#12216 = ORIENTED_EDGE ( 'NONE', *, *, #15945, .T. ) ;
#12217 = DIRECTION ( 'NONE',  ( 1.000000000000000000, 0.000000000000000000, 0.000000000000000000 ) ) ;
#12218 = B_SPLINE_CURVE_WITH_KNOTS ( 'NONE', 3,
 ( #2368, #874, #16555, #13077, #11946, #19171 ),
 .UNSPECIFIED., .F., .F.,
 ( 4, 2, 4 ),
 ( 2.321268216997094965E-07, 0.001878622960950495756, 0.003757013795079291486 ),
 .UNSPECIFIED. ) ;
#12219 = CARTESIAN_POINT ( 'NONE',  ( 3.846120219227944670, 3.114526743279256049, -11.34374999795161543 ) ) ;
#12220 = EDGE_CURVE ( 'NONE', #19560, #4381, #5001, .T. ) ;
#12221 = ORIENTED_EDGE ( 'NONE', *, *, #18616, .F. ) ;
#12222 = CARTESIAN_POINT ( 'NONE',  ( 8.843749997951615427, -2.873153789725853002, 3.954556930911842016 ) ) ;
#12223 = DIRECTION ( 'NONE',  ( 1.000000000000000000, 0.000000000000000000, 0.000000000000000000 ) ) ;
#12224 = AXIS2_PLACEMENT_3D ( 'NONE', #17004, #792, #6864 ) ;
#12225 = VERTEX_POINT ( 'NONE', #9011 ) ;
#12226 = AXIS2_PLACEMENT_3D ( 'NONE', #13768, #10577, #6246 ) ;
#12227 = CIRCLE ( 'NONE', #19241, 28.06981291497571007 ) ;
#12228 = LINE ( 'NONE', #4718, #17316 ) ;
#12229 = CARTESIAN_POINT ( 'NONE',  ( -16.96448111170888851, 1.130229351527647808, -35.00000000000000000 ) ) ;
#12230 = ORIENTED_EDGE ( 'NONE', *, *, #14059, .T. ) ;
#12231 = B_SPLINE_CURVE_WITH_KNOTS ( 'NONE', 3,
 ( #1477, #18671, #7663, #7769, #16688, #15289 ),
 .UNSPECIFIED., .F., .F.,
 ( 4, 2, 4 ),
 ( 2.321268216997199256E-07, 0.001878622960950494455, 0.003757013795079288884 ),
 .UNSPECIFIED. ) ;
#12232 = CARTESIAN_POINT ( 'NONE',  ( 7.843749997951614539, 4.781284448697194378, -1.016293382781411569 ) ) ;
#12233 = CARTESIAN_POINT ( 'NONE',  ( 12.73273607671833929, 4.522548057701235358, 1.899256020376435927 ) ) ;
#12234 = B_SPLINE_CURVE_WITH_KNOTS ( 'NONE', 3,
 ( #18289, #272, #18577, #6449, #9583, #17183 ),
 .UNSPECIFIED., .F., .F.,
 ( 4, 2, 4 ),
 ( 4.462636695616422376E-07, 0.001879885036799763083, 0.003759323809929964420 ),
 .UNSPECIFIED. ) ;
#12235 = ORIENTED_EDGE ( 'NONE', *, *, #1125, .T. ) ;
#12236 = EDGE_CURVE ( 'NONE', #12259, #6178, #10324, .T. ) ;
#12237 = CYLINDRICAL_SURFACE ( 'NONE', #10244, 28.06981291497571362 ) ;
#12238 = ORIENTED_EDGE ( 'NONE', *, *, #465, .T. ) ;
#12239 = CARTESIAN_POINT ( 'NONE',  ( 0.006974674093433516284, 24.42374957165205629, -2.249040938978583259 ) ) ;
#12240 = CIRCLE ( 'NONE', #13496, 7.500000000000000000 ) ;
#12241 = ORIENTED_EDGE ( 'NONE', *, *, #1674, .F. ) ;
#12242 = CARTESIAN_POINT ( 'NONE',  ( 2.765633920072236407, 2.336989772644613161, -24.63872515616080250 ) ) ;
#12243 = CARTESIAN_POINT ( 'NONE',  ( 12.00000000000000355, 0.000000000000000000, 0.000000000000000000 ) ) ;
#12244 = DIRECTION ( 'NONE',  ( 0.000000000000000000, 0.000000000000000000, 1.000000000000000000 ) ) ;
#12245 = DIRECTION ( 'NONE',  ( 0.000000000000000000, 0.000000000000000000, 1.000000000000000000 ) ) ;
#12246 = ADVANCED_FACE ( 'NONE', ( #18117, #1410 ), #11914, .T. ) ;
#12247 = AXIS2_PLACEMENT_3D ( 'NONE', #12056, #39, #1546 ) ;
#12248 = LINE ( 'NONE', #9242, #8878 ) ;
#12249 = ORIENTED_EDGE ( 'NONE', *, *, #2710, .F. ) ;
#12250 = CARTESIAN_POINT ( 'NONE',  ( 2.765633920072238183, -5.391175441198789109, 24.15498966839961170 ) ) ;
#12251 = EDGE_CURVE ( 'NONE', #2365, #9647, #5993, .T. ) ;
#12252 = PRESENTATION_LAYER_ASSIGNMENT (  '', '', ( #9705 ) ) ;
#12253 = VERTEX_POINT ( 'NONE', #13710 ) ;
#12254 = DIRECTION ( 'NONE',  ( -0.8660254037844363761, 0.5000000000000039968, 0.000000000000000000 ) ) ;
#12255 = DIRECTION ( 'NONE',  ( -1.000000000000000000, -0.000000000000000000, 0.000000000000000000 ) ) ;
#12256 = VERTEX_POINT ( 'NONE', #18024 ) ;
#12257 = DIRECTION ( 'NONE',  ( -1.000000000000000000, 0.000000000000000000, 0.000000000000000000 ) ) ;
#12258 = CARTESIAN_POINT ( 'NONE',  ( 4.620319390059819398, -1.773574444220757274, -10.96874999795161720 ) ) ;
#12259 = VERTEX_POINT ( 'NONE', #19611 ) ;
#12260 = CARTESIAN_POINT ( 'NONE',  ( -1.773574444220725077, 4.620319390059829168, -6.968749997951614539 ) ) ;
#12261 = ORIENTED_EDGE ( 'NONE', *, *, #9329, .T. ) ;
#12262 = DIRECTION ( 'NONE',  ( 1.000000000000000000, 0.000000000000000000, 0.000000000000000000 ) ) ;
#12263 = DIRECTION ( 'NONE',  ( 1.000000000000000000, 0.000000000000000000, 0.000000000000000000 ) ) ;
#12264 = ORIENTED_EDGE ( 'NONE', *, *, #15178, .T. ) ;
#12265 = VERTEX_POINT ( 'NONE', #13405 ) ;
#12266 = CARTESIAN_POINT ( 'NONE',  ( 0.5321745087963408727, 11.58891744060107065, 24.44564404695848836 ) ) ;
#12267 =( GEOMETRIC_REPRESENTATION_CONTEXT ( 3 ) GLOBAL_UNCERTAINTY_ASSIGNED_CONTEXT ( ( #2573 ) ) GLOBAL_UNIT_ASSIGNED_CONTEXT ( ( #5287, #12898, #17888 ) ) REPRESENTATION_CONTEXT ( 'NONE', 'WORKASPACE' ) );
#12268 = CARTESIAN_POINT ( 'NONE',  ( -2.444050593749990785, 4.233219804643887585, -6.843749997951615427 ) ) ;
#12269 = ORIENTED_EDGE ( 'NONE', *, *, #8664, .T. ) ;
#12270 = EDGE_CURVE ( 'NONE', #14758, #6823, #570, .T. ) ;
#12271 = EDGE_CURVE ( 'NONE', #7096, #17509, #2462, .T. ) ;
#12272 = SURFACE_SIDE_STYLE ('',( #6154 ) ) ;
#12273 = CONICAL_SURFACE ( 'NONE', #8125, 7.937500000000000000, 1.047197551196596521 ) ;
#12274 = B_SPLINE_CURVE_WITH_KNOTS ( 'NONE', 3,
 ( #15651, #242, #3238, #7738, #10754, #1842 ),
 .UNSPECIFIED., .F., .F.,
 ( 4, 2, 4 ),
 ( 4.462636677693390501E-07, 0.001879885020955137558, 0.003759323778242505774 ),
 .UNSPECIFIED. ) ;
#12275 = ORIENTED_EDGE ( 'NONE', *, *, #3006, .F. ) ;
#12276 = ADVANCED_FACE ( 'NONE', ( #12114 ), #18217, .F. ) ;
#12277 = CIRCLE ( 'NONE', #1451, 3.968750000000000000 ) ;
#12278 = CARTESIAN_POINT ( 'NONE',  ( 6.626241948324199882, -16.73597674598852691, -32.00000000000000000 ) ) ;
#12279 = DIRECTION ( 'NONE',  ( 0.000000000000000000, 1.224646799147333486E-16, 1.000000000000000000 ) ) ;
#12280 = CARTESIAN_POINT ( 'NONE',  ( 0.9027913098498173694, -5.700000000000006395, -11.81249999590322552 ) ) ;
#12281 = ADVANCED_FACE ( 'NONE', ( #8710 ), #17916, .T. ) ;
#12282 = ORIENTED_EDGE ( 'NONE', *, *, #16350, .F. ) ;
#12283 = VERTEX_POINT ( 'NONE', #8812 ) ;
#12284 = DIRECTION ( 'NONE',  ( 0.000000000000000000, 0.000000000000000000, 1.000000000000000000 ) ) ;
#12285 = SURFACE_SIDE_STYLE ('',( #19580 ) ) ;
#12286 = EDGE_CURVE ( 'NONE', #9970, #18497, #11440, .T. ) ;
#12287 = FACE_OUTER_BOUND ( 'NONE', #6102, .T. ) ;
#12288 = AXIS2_PLACEMENT_3D ( 'NONE', #2404, #3909, #10031 ) ;
#12289 = ORIENTED_EDGE ( 'NONE', *, *, #18222, .T. ) ;
#12290 = CARTESIAN_POINT ( 'NONE',  ( 13.00000000000000000, -5.567819778318897406, -1.220402768007724292 ) ) ;
#12291 = LINE ( 'NONE', #18094, #2344 ) ;
#12292 = FACE_OUTER_BOUND ( 'NONE', #7082, .T. ) ;
#12293 = CARTESIAN_POINT ( 'NONE',  ( 2.171938186095908829, 23.93436800624300886, 12.96259772325185544 ) ) ;
#12294 = CIRCLE ( 'NONE', #8462, 1.000000000000002442 ) ;
#12295 = CARTESIAN_POINT ( 'NONE',  ( -0.9027913098498572264, 5.699999999999999289, -10.50000000000000711 ) ) ;
#12296 = ORIENTED_EDGE ( 'NONE', *, *, #3425, .F. ) ;
#12297 = CARTESIAN_POINT ( 'NONE',  ( 2.789999999999999147, 2.680914349914567470E-13, -25.59481291497571220 ) ) ;
#12298 = DIRECTION ( 'NONE',  ( 0.000000000000000000, 0.000000000000000000, -1.000000000000000000 ) ) ;
#12299 = ORIENTED_EDGE ( 'NONE', *, *, #11743, .F. ) ;
#12300 = LINE ( 'NONE', #12595, #9444 ) ;
#12301 = AXIS2_PLACEMENT_3D ( 'NONE', #14094, #15408, #18694 ) ;
#12302 = EDGE_CURVE ( 'NONE', #17067, #17625, #4606, .T. ) ;
#12303 = LINE ( 'NONE', #8080, #12808 ) ;
#12304 = CARTESIAN_POINT ( 'NONE',  ( 9.968749997951615427, 0.2590123213421660631, -4.942249507334554259 ) ) ;
#12305 = CARTESIAN_POINT ( 'NONE',  ( 2.789999999999999147, -23.48180575137726223, -5.535312321042966666 ) ) ;
#12306 = EDGE_LOOP ( 'NONE', ( #19730, #13542, #6561, #1633 ) ) ;
#12307 = EDGE_CURVE ( 'NONE', #9684, #4759, #12003, .T. ) ;
#12308 = AXIS2_PLACEMENT_3D ( 'NONE', #18539, #12914, #9448 ) ;
#12309 = LINE ( 'NONE', #12407, #6582 ) ;
#12310 =( NAMED_UNIT ( * ) SI_UNIT ( $, .STERADIAN. ) SOLID_ANGLE_UNIT ( ) );
#12311 = DIRECTION ( 'NONE',  ( 1.000000000000000000, 0.000000000000000000, 0.000000000000000000 ) ) ;
#12312 = EDGE_CURVE ( 'NONE', #15601, #6013, #4399, .T. ) ;
#12313 = CARTESIAN_POINT ( 'NONE',  ( 9.000000000000001776, 1.102182119232617911E-15, -30.00000000000000355 ) ) ;
#12314 = ORIENTED_EDGE ( 'NONE', *, *, #16337, .F. ) ;
#12315 =( BOUNDED_SURFACE ( )  B_SPLINE_SURFACE ( 1, 2, ( 
 ( #14464, #12962, #12860, #18956, #19055, #5247, #5344, #17560, #3847, #8741, #14659, #7123, #8941, #19531, #5826, #1235, #8844 ),
 ( #3947, #13338, #19244, #13539, #11941, #13253, #4339, #14943, #7315, #17656, #14751, #8644, #5630, #18052, #947, #19641, #1144 ) ),
 .UNSPECIFIED., .F., .F., .F. ) 
 B_SPLINE_SURFACE_WITH_KNOTS ( ( 2, 2 ),
 ( 3, 2, 2, 2, 2, 2, 2, 2, 3 ),
 ( 0.000000000000000000, 1.000000000000000000 ),
 ( 0.000000000000000000, 0.05000000000000000278, 0.1000000000000000056, 0.1499999999999999944, 0.2000000000000000111, 0.2500000000000000000, 0.2999999999999999889, 0.3499999999999999778, 0.4000000000000000222 ),
 .UNSPECIFIED. ) 
 GEOMETRIC_REPRESENTATION_ITEM ( )  RATIONAL_B_SPLINE_SURFACE ( (
 ( 1.000000000000000000, 0.9876883405951377704, 1.000000000000000000, 0.9876883405951377704, 1.000000000000000000, 0.9876883405951377704, 1.000000000000000000, 0.9876883405951377704, 1.000000000000000000, 0.9876883405951377704, 1.000000000000000000, 0.9876883405951377704, 1.000000000000000000, 0.9876883405951377704, 1.000000000000000000, 0.9876883405951377704, 1.000000000000000000),
 ( 1.000000000000000000, 0.9876883405951377704, 1.000000000000000000, 0.9876883405951377704, 1.000000000000000000, 0.9876883405951377704, 1.000000000000000000, 0.9876883405951377704, 1.000000000000000000, 0.9876883405951377704, 1.000000000000000000, 0.9876883405951377704, 1.000000000000000000, 0.9876883405951377704, 1.000000000000000000, 0.9876883405951377704, 1.000000000000000000) ) ) 
 REPRESENTATION_ITEM ( '' )  SURFACE ( )  );
#12316 = CARTESIAN_POINT ( 'NONE',  ( -90.00000000000000000, 0.000000000000000000, -9.000000000000021316 ) ) ;
#12317 = LINE ( 'NONE', #16249, #18953 ) ;
#12318 = CARTESIAN_POINT ( 'NONE',  ( 0.000000000000000000, 4.070113636966254069E-16, 3.323500000000020993 ) ) ;
#12319 = CARTESIAN_POINT ( 'NONE',  ( 1.394999999999999574, -12.52377138324206740, -25.12109765559666741 ) ) ;
#12320 = ORIENTED_EDGE ( 'NONE', *, *, #12772, .T. ) ;
#12321 = CARTESIAN_POINT ( 'NONE',  ( 2.783025306068356297, 16.17543236988015209, -18.43727551351014071 ) ) ;
#12322 = EDGE_CURVE ( 'NONE', #12535, #4037, #10156, .T. ) ;
#12323 = CARTESIAN_POINT ( 'NONE',  ( 1.394999999999999574, -27.76164181293054511, 4.147968289691193355 ) ) ;
#12324 = EDGE_LOOP ( 'NONE', ( #17095, #8117, #4821, #13364 ) ) ;
#12325 = CARTESIAN_POINT ( 'NONE',  ( -11.00000000000000355, -4.898587196589412829E-16, 0.000000000000000000 ) ) ;
#12326 = DIRECTION ( 'NONE',  ( -1.000000000000000000, 0.000000000000000000, 0.000000000000000000 ) ) ;
#12327 = VECTOR ( 'NONE', #2078, 1000.000000000000000 ) ;
#12328 = EDGE_LOOP ( 'NONE', ( #10882, #3884, #6957, #13551 ) ) ;
#12329 = CIRCLE ( 'NONE', #2415, 1.000000000000002665 ) ;
#12330 = DIRECTION ( 'NONE',  ( 0.4330127018922180770, -0.7500000000000021094, 0.4999999999999979461 ) ) ;
#12331 = CARTESIAN_POINT ( 'NONE',  ( 4.888101187499994893, -0.7741991708319229115, -7.343749997951615427 ) ) ;
#12332 = ORIENTED_EDGE ( 'NONE', *, *, #11679, .F. ) ;
#12333 = CYLINDRICAL_SURFACE ( 'NONE', #11697, 9.000000000000000000 ) ;
#12334 = DIRECTION ( 'NONE',  ( 0.000000000000000000, 0.000000000000000000, 1.000000000000000000 ) ) ;
#12335 = EDGE_CURVE ( 'NONE', #8958, #18746, #9113, .T. ) ;
#12336 = VERTEX_POINT ( 'NONE', #15216 ) ;
#12337 = CYLINDRICAL_SURFACE ( 'NONE', #4790, 2.524999999999995914 ) ;
#12338 = VERTEX_POINT ( 'NONE', #19410 ) ;
#12339 = DIRECTION ( 'NONE',  ( 1.000000000000000000, 0.000000000000000000, 0.000000000000000000 ) ) ;
#12340 = VERTEX_POINT ( 'NONE', #14914 ) ;
#12341 = CARTESIAN_POINT ( 'NONE',  ( 8.000000000000000000, 0.000000000000000000, 0.000000000000000000 ) ) ;
#12342 = CIRCLE ( 'NONE', #9151, 4.000000000000000000 ) ;
#12343 = CARTESIAN_POINT ( 'NONE',  ( 15.19790265903627358, 9.644882309621939598, 35.00000000000000000 ) ) ;
#12344 = DIRECTION ( 'NONE',  ( 0.000000000000000000, 0.000000000000000000, 1.000000000000000000 ) ) ;
#12345 = CARTESIAN_POINT ( 'NONE',  ( 8.968749997951613651, 4.780397808154257078, 1.280903732194454303 ) ) ;
#12346 = VERTEX_POINT ( 'NONE', #1208 ) ;
#12347 = CARTESIAN_POINT ( 'NONE',  ( 0.4314184204727332661, 23.43037373958377501, 12.94152279942384709 ) ) ;
#12348 = DIRECTION ( 'NONE',  ( -1.000000000000000000, -0.000000000000000000, -0.000000000000000000 ) ) ;
#12349 = EDGE_CURVE ( 'NONE', #18565, #2110, #7284, .T. ) ;
#12350 = CIRCLE ( 'NONE', #11391, 1.000000000000000000 ) ;
#12351 = EDGE_LOOP ( 'NONE', ( #18431, #18349, #12775, #3104 ) ) ;
#12352 = CIRCLE ( 'NONE', #4053, 7.800000000000000711 ) ;
#12353 = DIRECTION ( 'NONE',  ( -0.5000000000000039968, -0.8660254037844363761, 0.000000000000000000 ) ) ;
#12354 = CARTESIAN_POINT ( 'NONE',  ( -0.5958122406255600412, 5.668774803599166745, 0.000000000000000000 ) ) ;
#12355 = ADVANCED_BREP_SHAPE_REPRESENTATION ( '', ( #15876, #16724 ), #7108 ) ;
#12356 = ORIENTED_EDGE ( 'NONE', *, *, #12124, .T. ) ;
#12357 = DIRECTION ( 'NONE',  ( 1.000000000000000000, 0.000000000000000000, 0.000000000000000000 ) ) ;
#12358 = CARTESIAN_POINT ( 'NONE',  ( 13.34374999795161365, 4.150607464521828938, -2.695436003842674566 ) ) ;
#12359 = ADVANCED_FACE ( 'NONE', ( #18798, #6188 ), #14200, .F. ) ;
#12360 =( NAMED_UNIT ( * ) SI_UNIT ( $, .STERADIAN. ) SOLID_ANGLE_UNIT ( ) );
#12361 = VERTEX_POINT ( 'NONE', #9308 ) ;
#12362 = CARTESIAN_POINT ( 'NONE',  ( 0.0001048950922011769414, -20.67847077765692632, -12.51925356660783351 ) ) ;
#12363 = EDGE_LOOP ( 'NONE', ( #19339, #17659, #6026, #5066 ) ) ;
#12364 = CARTESIAN_POINT ( 'NONE',  ( -13.86923836996420967, -11.47363181547641275, 32.00000000000000000 ) ) ;
#12365 = DIRECTION ( 'NONE',  ( 0.000000000000000000, 0.000000000000000000, -1.000000000000000000 ) ) ;
#12366 = ORIENTED_EDGE ( 'NONE', *, *, #9471, .T. ) ;
#12367 = ORIENTED_EDGE ( 'NONE', *, *, #13201, .F. ) ;
#12368 = CARTESIAN_POINT ( 'NONE',  ( 0.000000000000000000, 24.04302995059966364, -1.991882183130399664 ) ) ;
#12369 = CIRCLE ( 'NONE', #11071, 8.239200000000002078 ) ;
#12370 = CARTESIAN_POINT ( 'NONE',  ( -0.3020334839682480288, 5.763142191869157216, -8.812499995903225525 ) ) ;
#12371 = ORIENTED_EDGE ( 'NONE', *, *, #8748, .T. ) ;
#12372 = DIRECTION ( 'NONE',  ( 1.000000000000000000, 0.000000000000000000, 0.000000000000000000 ) ) ;
#12373 = EDGE_CURVE ( 'NONE', #3605, #1752, #18697, .T. ) ;
#12374 = ORIENTED_EDGE ( 'NONE', *, *, #9084, .F. ) ;
#12375 = CIRCLE ( 'NONE', #3753, 4.200000000000000178 ) ;
#12376 = EDGE_CURVE ( 'NONE', #7834, #4794, #9412, .T. ) ;
#12377 = CARTESIAN_POINT ( 'NONE',  ( -5.209999999999999964, 0.000000000000000000, 0.000000000000000000 ) ) ;
#12378 = CARTESIAN_POINT ( 'NONE',  ( 8.843749997951615427, 1.988169868018562436, 4.465502636338039011 ) ) ;
#12379 = CARTESIAN_POINT ( 'NONE',  ( 2.718131853594929037, -12.74240566898999383, 21.92302674874958868 ) ) ;
#12380 = EDGE_CURVE ( 'NONE', #2597, #12952, #5519, .T. ) ;
#12381 = ORIENTED_EDGE ( 'NONE', *, *, #985, .F. ) ;
#12382 = EDGE_LOOP ( 'NONE', ( #9278, #2912, #8153, #15364 ) ) ;
#12383 = CARTESIAN_POINT ( 'NONE',  ( -11.00000000000000355, 4.215373648918918192, 3.375000000000000888 ) ) ;
#12384 = CARTESIAN_POINT ( 'NONE',  ( 5.700000000000001066, -4.360680574150373717E-16, -12.66727757604273386 ) ) ;
#12385 = VERTEX_POINT ( 'NONE', #11003 ) ;
#12386 = ORIENTED_EDGE ( 'NONE', *, *, #7445, .F. ) ;
#12387 = CYLINDRICAL_SURFACE ( 'NONE', #17841, 13.19999999999999929 ) ;
#12388 = CARTESIAN_POINT ( 'NONE',  ( -5.763142191869158992, -0.3020334839682081163, -13.81249999590322552 ) ) ;
#12389 = DIRECTION ( 'NONE',  ( 1.000000000000000000, 6.419766481290786633E-33, -0.000000000000000000 ) ) ;
#12390 = EDGE_CURVE ( 'NONE', #15288, #10168, #2918, .T. ) ;
#12391 = CARTESIAN_POINT ( 'NONE',  ( -2.000000000000001776, 0.000000000000000000, 0.000000000000000000 ) ) ;
#12392 = AXIS2_PLACEMENT_3D ( 'NONE', #4496, #16613, #18313 ) ;
#12393 = CARTESIAN_POINT ( 'NONE',  ( -1.886022603841227552, 0.000000000000000000, 0.000000000000000000 ) ) ;
#12394 = VECTOR ( 'NONE', #2151, 1000.000000000000000 ) ;
#12395 = VERTEX_POINT ( 'NONE', #6476 ) ;
#12396 = CARTESIAN_POINT ( 'NONE',  ( 8.843749997951615427, -1.988169868018530462, -4.465502636338051445 ) ) ;
#12397 = DIRECTION ( 'NONE',  ( 0.000000000000000000, 1.224646799147353207E-16, 1.000000000000000000 ) ) ;
#12398 = VERTEX_POINT ( 'NONE', #17205 ) ;
#12399 = CARTESIAN_POINT ( 'NONE',  ( -30.00000000000000000, 6.000000000000000888, 0.000000000000000000 ) ) ;
#12401 = EDGE_CURVE ( 'NONE', #639, #18135, #11452, .T. ) ;
#12400 = ADVANCED_FACE ( 'NONE', ( #10809 ), #15906, .T. ) ;
#12402 = CARTESIAN_POINT ( 'NONE',  ( -20.63749999999999574, 8.327598234201999146E-16, 6.799999999999998046 ) ) ;
#12403 = DIRECTION ( 'NONE',  ( -5.011428603230760289E-33, 0.7806247497997995666, 0.6250000000000001110 ) ) ;
#12404 = CARTESIAN_POINT ( 'NONE',  ( -2.000000000000001776, -3.218695387886215009, -3.000000000000002220 ) ) ;
#12405 = ORIENTED_EDGE ( 'NONE', *, *, #3432, .F. ) ;
#12406 = CIRCLE ( 'NONE', #14955, 10.00000000000000000 ) ;
#12407 = CARTESIAN_POINT ( 'NONE',  ( 11.58013454126452579, -14.56230589874905412, 32.00000000000000000 ) ) ;
#12408 = CARTESIAN_POINT ( 'NONE',  ( 12.32184790671639618, 13.12143529358541016, -35.00000000000000000 ) ) ;
#12409 = VECTOR ( 'NONE', #515, 1000.000000000000000 ) ;
#12410 = LINE ( 'NONE', #9605, #8322 ) ;
#12411 = ORIENTED_EDGE ( 'NONE', *, *, #13701, .F. ) ;
#12412 = CARTESIAN_POINT ( 'NONE',  ( -11.00000000000000355, -4.898587196589412829E-16, 0.000000000000000000 ) ) ;
#12413 = PLANE ( 'NONE',  #10338 ) ;
#12414 = CARTESIAN_POINT ( 'NONE',  ( 5.575441324182689229, -1.185096637661254171, -10.00000000000000533 ) ) ;
#12415 = CARTESIAN_POINT ( 'NONE',  ( -34.92499999999994742, 1.224646799147353256E-15, -10.00000000000000000 ) ) ;
#12416 = ORIENTED_EDGE ( 'NONE', *, *, #14058, .T. ) ;
#12417 = DIRECTION ( 'NONE',  ( -1.000000000000000000, -0.000000000000000000, -0.000000000000000000 ) ) ;
#12418 = DIRECTION ( 'NONE',  ( 0.000000000000000000, 0.000000000000000000, 1.000000000000000000 ) ) ;
#12419 = ORIENTED_EDGE ( 'NONE', *, *, #3552, .F. ) ;
#12420 = DIRECTION ( 'NONE',  ( 1.000000000000000000, -0.000000000000000000, -0.000000000000000000 ) ) ;
#12421 = CARTESIAN_POINT ( 'NONE',  ( 0.000000000000000000, 0.000000000000000000, 0.000000000000000000 ) ) ;
#12422 = AXIS2_PLACEMENT_3D ( 'NONE', #18480, #6169, #10784 ) ;
#12423 = ORIENTED_EDGE ( 'NONE', *, *, #9986, .T. ) ;
#12424 = DIRECTION ( 'NONE',  ( -1.000000000000000000, -0.000000000000000000, -0.000000000000000000 ) ) ;
#12425 = CARTESIAN_POINT ( 'NONE',  ( 8.812499995903225525, 2.620002426024544029, -5.142044285764751699 ) ) ;
#12426 =( BOUNDED_CURVE ( )  B_SPLINE_CURVE ( 2, ( #10916, #17020, #3309, #17119, #9423, #308, #6389, #13719, #18611, #12910, #2006, #611, #2297, #8507, #8104 ),
 .UNSPECIFIED., .F., .F. ) 
 B_SPLINE_CURVE_WITH_KNOTS ( ( 3, 2, 2, 2, 2, 2, 2, 3 ),
 ( 0.000000000000000000, 0.04999999999999999584, 0.09999999999999999167, 0.1499999999999999944, 0.1999999999999999833, 0.2500000000000000000, 0.2999999999999999889, 0.3499999999999999778 ),
 .UNSPECIFIED. ) 
 CURVE ( )  GEOMETRIC_REPRESENTATION_ITEM ( )  RATIONAL_B_SPLINE_CURVE ( ( 1.000000000000000000, 0.9876883405951377704, 1.000000000000000000, 0.9876883405951377704, 1.000000000000000000, 0.9876883405951377704, 1.000000000000000000, 0.9876883405951377704, 1.000000000000000000, 0.9876883405951377704, 1.000000000000000000, 0.9876883405951377704, 1.000000000000000000, 0.9876883405951377704, 1.000000000000000000 ) ) 
 REPRESENTATION_ITEM ( '' )  );
#12427 = ORIENTED_EDGE ( 'NONE', *, *, #3622, .T. ) ;
#12428 = DIRECTION ( 'NONE',  ( 0.000000000000000000, 0.000000000000000000, 1.000000000000000000 ) ) ;
#12429 = CARTESIAN_POINT ( 'NONE',  ( -7.937500000000000000, -4.582717761692662428, -6.527800000000000047 ) ) ;
#12430 = ORIENTED_EDGE ( 'NONE', *, *, #11951, .T. ) ;
#12431 = LINE ( 'NONE', #529, #3522 ) ;
#12432 = ORIENTED_EDGE ( 'NONE', *, *, #14032, .T. ) ;
#12434 = CARTESIAN_POINT ( 'NONE',  ( 5.575441324182689229, -1.185096637661254171, -11.31249999590322375 ) ) ;
#12433 = AXIS2_PLACEMENT_3D ( 'NONE', #15807, #6022, #10542 ) ;
#12435 = ORIENTED_EDGE ( 'NONE', *, *, #15249, .F. ) ;
#12436 = DIRECTION ( 'NONE',  ( 1.000000000000000000, 0.000000000000000000, 0.000000000000000000 ) ) ;
#12437 = CARTESIAN_POINT ( 'NONE',  ( -0.5109457054262123155, -4.861323657744403448, -8.843749997951615427 ) ) ;
#12438 = CARTESIAN_POINT ( 'NONE',  ( -3.631840208645857437, -4.484949146646330931, -6.500000000000005329 ) ) ;
#12439 = CARTESIAN_POINT ( 'NONE',  ( 0.02436607992776541887, 12.59161484032942901, -21.30679549418617924 ) ) ;
#12440 = PRODUCT_DEFINITION_FORMATION_WITH_SPECIFIED_SOURCE ( 'ANY', '', #5221, .NOT_KNOWN. ) ;
#12441 = ORIENTED_EDGE ( 'NONE', *, *, #1149, .F. ) ;
#12442 = CARTESIAN_POINT ( 'NONE',  ( 2.789999999999999147, -7.334849878007672963, 23.31896751603329676 ) ) ;
#12443 = EDGE_CURVE ( 'NONE', #18676, #16730, #14002, .T. ) ;
#12444 = CARTESIAN_POINT ( 'NONE',  ( 0.000000000000000000, 0.000000000000000000, 10.00000000000000000 ) ) ;
#12445 = AXIS2_PLACEMENT_3D ( 'NONE', #11372, #9976, #955 ) ;
#12446 = ORIENTED_EDGE ( 'NONE', *, *, #3486, .T. ) ;
#12447 = CARTESIAN_POINT ( 'NONE',  ( 2.257825467309741541, 3.467596033028661928, -26.83036154824990760 ) ) ;
#12448 = FACE_OUTER_BOUND ( 'NONE', #11043, .T. ) ;
#12449 = ORIENTED_EDGE ( 'NONE', *, *, #14267, .F. ) ;
#12451 = CARTESIAN_POINT ( 'NONE',  ( 2.030753616560877717, 12.05220173035473863, -24.80264696524870516 ) ) ;
#12450 = AXIS2_PLACEMENT_3D ( 'NONE', #7119, #17557, #4042 ) ;
#12452 = CARTESIAN_POINT ( 'NONE',  ( 12.84374999795161543, 3.632567103900569361, -3.270778111535288080 ) ) ;
#12453 = ORIENTED_EDGE ( 'NONE', *, *, #13163, .F. ) ;
#12454 = DIRECTION ( 'NONE',  ( 0.000000000000000000, 0.000000000000000000, 1.000000000000000000 ) ) ;
#12455 = EDGE_LOOP ( 'NONE', ( #5122, #8997, #11945, #1600 ) ) ;
#12456 = PRODUCT_CONTEXT ( 'NONE', #19276, 'mechanical' ) ;
#12457 = DIRECTION ( 'NONE',  ( 1.000000000000000000, 1.224646799147353207E-16, 0.000000000000000000 ) ) ;
#12458 = DIRECTION ( 'NONE',  ( 0.000000000000000000, 0.000000000000000000, 1.000000000000000000 ) ) ;
#12459 = ORIENTED_EDGE ( 'NONE', *, *, #1010, .F. ) ;
#12460 = EDGE_CURVE ( 'NONE', #19497, #5656, #10494, .T. ) ;
#12461 = ORIENTED_EDGE ( 'NONE', *, *, #8851, .F. ) ;
#12462 = DIRECTION ( 'NONE',  ( 0.000000000000000000, 0.000000000000000000, -1.000000000000000000 ) ) ;
#12463 = CARTESIAN_POINT ( 'NONE',  ( 4.861323657744407001, -0.5109457054261775655, -13.84374999795161543 ) ) ;
#12464 = VERTEX_POINT ( 'NONE', #4702 ) ;
#12465 = STYLED_ITEM ( 'NONE', ( #15346 ), #16364 ) ;
#12466 = AXIS2_PLACEMENT_3D ( 'NONE', #7306, #12137, #15241 ) ;
#12467 = ADVANCED_FACE ( 'NONE', ( #7890 ), #14098, .T. ) ;
#12468 = DIRECTION ( 'NONE',  ( 0.000000000000000000, 0.000000000000000000, -1.000000000000000000 ) ) ;
#12469 = EDGE_LOOP ( 'NONE', ( #12977, #1000, #8545, #2958 ) ) ;
#12470 = DIRECTION ( 'NONE',  ( 0.000000000000000000, 0.000000000000000000, -1.000000000000000000 ) ) ;
#12471 = DIRECTION ( 'NONE',  ( 0.000000000000000000, -0.000000000000000000, -1.000000000000000000 ) ) ;
#12472 = DIRECTION ( 'NONE',  ( -1.000000000000000000, 0.000000000000000000, -0.000000000000000000 ) ) ;
#12473 = ORIENTED_EDGE ( 'NONE', *, *, #3767, .T. ) ;
#12474 = AXIS2_PLACEMENT_3D ( 'NONE', #2640, #18062, #11755 ) ;
#12475 = CARTESIAN_POINT ( 'NONE',  ( -15.00000000000000355, 4.874999999999998224, 3.903123748998998721 ) ) ;
#12476 = CIRCLE ( 'NONE', #19493, 1.000000000000004441 ) ;
#12477 = B_SPLINE_CURVE_WITH_KNOTS ( 'NONE', 3,
 ( #16639, #4628, #4522, #23, #10637, #9135, #2916, #12139 ),
 .UNSPECIFIED., .F., .F.,
 ( 4, 2, 2, 4 ),
 ( 0.004637198101876895302, 0.005792104118025203502, 0.006947010134173512569, 0.009256822166470130703 ),
 .UNSPECIFIED. ) ;
#12478 = VERTEX_POINT ( 'NONE', #13908 ) ;
#12479 = EDGE_CURVE ( 'NONE', #14825, #2982, #10801, .T. ) ;
#12480 = ORIENTED_EDGE ( 'NONE', *, *, #5716, .F. ) ;
#12481 = CARTESIAN_POINT ( 'NONE',  ( 2.849999999999954348, -4.936344801571327601, -7.312499995903225525 ) ) ;
#12482 = EDGE_CURVE ( 'NONE', #15544, #11752, #1860, .T. ) ;
#12483 = CARTESIAN_POINT ( 'NONE',  ( 0.000000000000000000, 15.74360496233383522, 18.28042085475283329 ) ) ;
#12484 = CARTESIAN_POINT ( 'NONE',  ( -20.63749999999999929, 0.000000000000000000, -4.000000000000000000 ) ) ;
#12485 = CARTESIAN_POINT ( 'NONE',  ( 111.3234999999999957, 0.000000000000000000, 4.000000000000000000 ) ) ;
#12486 = EDGE_CURVE ( 'NONE', #13382, #10991, #10164, .T. ) ;
#12487 = CARTESIAN_POINT ( 'NONE',  ( 4.611396867937200383, 3.350375938067097881, -14.00000000000000533 ) ) ;
#12488 = EDGE_LOOP ( 'NONE', ( #9524, #3473, #14456, #876 ) ) ;
#12489 = CYLINDRICAL_SURFACE ( 'NONE', #1972, 2.524999999999996358 ) ;
#12490 = EDGE_CURVE ( 'NONE', #12395, #1207, #15702, .T. ) ;
#12491 = CARTESIAN_POINT ( 'NONE',  ( 6.843749997951615427, -3.413342815706642518E-14, 4.888101187500000222 ) ) ;
#12492 = VECTOR ( 'NONE', #1549, 1000.000000000000000 ) ;
#12493 = ORIENTED_EDGE ( 'NONE', *, *, #6847, .T. ) ;
#12494 = CARTESIAN_POINT ( 'NONE',  ( -18.68117051311639543, -3.372863662543042818, -32.00000000000000000 ) ) ;
#12495 = CARTESIAN_POINT ( 'NONE',  ( 14.84374999795161543, 1.988169868018623720, -4.465502636338010589 ) ) ;
#12496 = CARTESIAN_POINT ( 'NONE',  ( 16.28688694438835327, -7.664027248171309203, 35.00000000000000000 ) ) ;
#12497 = CARTESIAN_POINT ( 'NONE',  ( -7.723595606797438030E-14, -23.69897269326674305, -5.456611084822102775 ) ) ;
#12498 = EDGE_CURVE ( 'NONE', #6403, #12192, #10904, .T. ) ;
#12499 = CARTESIAN_POINT ( 'NONE',  ( 0.006930995026450773554, -23.92277630352799278, 5.408431875071351591 ) ) ;
#12500 = ORIENTED_EDGE ( 'NONE', *, *, #9981, .F. ) ;
#12501 = LINE ( 'NONE', #4600, #12991 ) ;
#12502 = CARTESIAN_POINT ( 'NONE',  ( -17.68117051311639898, -3.372863662543042818, -35.00000000000000000 ) ) ;
#12503 = CARTESIAN_POINT ( 'NONE',  ( -22.50000000000000711, 0.000000000000000000, 0.000000000000000000 ) ) ;
#12504 = ORIENTED_EDGE ( 'NONE', *, *, #16475, .T. ) ;
#12505 = CARTESIAN_POINT ( 'NONE',  ( 5.574407415329157622, -1.493657965219523209, -13.50000000000000533 ) ) ;
#12506 = CIRCLE ( 'NONE', #11236, 1.000000000000000888 ) ;
#12507 = CARTESIAN_POINT ( 'NONE',  ( -2.444050593750049849, -4.233219804643852946, -6.656249997951614539 ) ) ;
#12508 = AXIS2_PLACEMENT_3D ( 'NONE', #14730, #11234, #2417 ) ;
#12509 = ADVANCED_FACE ( 'NONE', ( #19092 ), #3886, .T. ) ;
#12510 = CARTESIAN_POINT ( 'NONE',  ( 14.00000000000000533, -2.318398865532073305, 5.207209108562820710 ) ) ;
#12511 = AXIS2_PLACEMENT_3D ( 'NONE', #9964, #2433, #8349 ) ;
#12512 = CYLINDRICAL_SURFACE ( 'NONE', #4717, 1.000000000000004441 ) ;
#12513 = ORIENTED_EDGE ( 'NONE', *, *, #12879, .F. ) ;
#12514 = CARTESIAN_POINT ( 'NONE',  ( 2.790000000000078639, 15.96555658743789152, -18.34439787333489136 ) ) ;
#12515 = APPLICATION_CONTEXT ( 'automotive_design' ) ;
#12516 = CARTESIAN_POINT ( 'NONE',  ( -1.510506337161861667, 4.648860486681953397, -10.84374999795161543 ) ) ;
#12517 = ORIENTED_EDGE ( 'NONE', *, *, #8685, .T. ) ;
#12518 = CARTESIAN_POINT ( 'NONE',  ( 13.84374999795161543, -3.954556930911842016, -2.873153789725852558 ) ) ;
#12519 = DIRECTION ( 'NONE',  ( 0.000000000000000000, 0.000000000000000000, -1.000000000000000000 ) ) ;
#12520 = ORIENTED_EDGE ( 'NONE', *, *, #14817, .F. ) ;
#12521 = CIRCLE ( 'NONE', #5164, 4.762499999999999289 ) ;
#12522 = AXIS2_PLACEMENT_3D ( 'NONE', #9618, #3412, #4811 ) ;
#12523 = EDGE_CURVE ( 'NONE', #6786, #12464, #14512, .T. ) ;
#12524 = VECTOR ( 'NONE', #7698, 1000.000000000000000 ) ;
#12525 = CARTESIAN_POINT ( 'NONE',  ( 1.749999999999998002, -20.02152543075360214, 19.67366047555523068 ) ) ;
#12526 = CARTESIAN_POINT ( 'NONE',  ( 13.00000000000000178, 4.920309236097874184, 1.604440756441510407 ) ) ;
#12527 = ORIENTED_EDGE ( 'NONE', *, *, #13159, .T. ) ;
#12528 = CARTESIAN_POINT ( 'NONE',  ( 5.476417968967387750, 17.43449690031536292, -32.00000000000000000 ) ) ;
#12529 = CARTESIAN_POINT ( 'NONE',  ( 0.7741991708318884946, 4.888101187500000222, -11.96874999795161365 ) ) ;
#12530 = ORIENTED_EDGE ( 'NONE', *, *, #12572, .F. ) ;
#12531 = DIRECTION ( 'NONE',  ( -0.000000000000000000, -0.000000000000000000, 1.000000000000000000 ) ) ;
#12532 = ORIENTED_EDGE ( 'NONE', *, *, #2734, .F. ) ;
#12533 = ADVANCED_FACE ( 'NONE', ( #3790 ), #18776, .T. ) ;
#12534 = DIRECTION ( 'NONE',  ( -0.000000000000000000, -0.000000000000000000, 1.000000000000000000 ) ) ;
#12535 = VERTEX_POINT ( 'NONE', #18896 ) ;
#12536 = EDGE_CURVE ( 'NONE', #22, #4727, #11117, .T. ) ;
#12537 = DIRECTION ( 'NONE',  ( -1.000000000000000000, -0.000000000000000000, -0.000000000000000000 ) ) ;
#12538 = CARTESIAN_POINT ( 'NONE',  ( -13.86923836996420967, -11.47363181547641275, -32.00000000000000000 ) ) ;
#12539 = CARTESIAN_POINT ( 'NONE',  ( 2.789999999999999147, 0.000000000000000000, 0.000000000000000000 ) ) ;
#12540 = CIRCLE ( 'NONE', #7393, 1.000000000000000888 ) ;
#12541 = AXIS2_PLACEMENT_3D ( 'NONE', #6343, #9475, #1764 ) ;
#12542 = DIRECTION ( 'NONE',  ( 0.000000000000000000, 0.000000000000000000, 1.000000000000000000 ) ) ;
#12543 = ORIENTED_EDGE ( 'NONE', *, *, #5053, .T. ) ;
#12544 = CIRCLE ( 'NONE', #13181, 7.800000000000000711 ) ;
#12545 = DIRECTION ( 'NONE',  ( 1.000000000000000000, -0.000000000000000000, -0.000000000000000000 ) ) ;
#12546 = CARTESIAN_POINT ( 'NONE',  ( 2.765633920072242624, 9.836394144775706394, 22.71065055754456097 ) ) ;
#12547 = VERTEX_POINT ( 'NONE', #799 ) ;
#12548 = AXIS2_PLACEMENT_3D ( 'NONE', #16103, #3987, #13284 ) ;
#12549 =( BOUNDED_SURFACE ( )  B_SPLINE_SURFACE ( 1, 2, ( 
 ( #7437, #17866, #19661, #7232, #13357, #7332, #11859, #13452, #17970, #4260, #5846, #10372, #19553, #16470, #14964, #11962, #18068 ),
 ( #4359, #10468, #2848, #10959, #4849, #3450, #10858, #1942, #17064, #5046, #11054, #1653, #12564, #1554, #17160, #18750, #6143 ) ),
 .UNSPECIFIED., .F., .F., .F. ) 
 B_SPLINE_SURFACE_WITH_KNOTS ( ( 2, 2 ),
 ( 3, 2, 2, 2, 2, 2, 2, 2, 3 ),
 ( 0.000000000000000000, 1.000000000000000000 ),
 ( 0.000000000000000000, 0.05000000000000000278, 0.1000000000000000056, 0.1499999999999999944, 0.2000000000000000111, 0.2500000000000000000, 0.2999999999999999889, 0.3499999999999999778, 0.4000000000000000222 ),
 .UNSPECIFIED. ) 
 GEOMETRIC_REPRESENTATION_ITEM ( )  RATIONAL_B_SPLINE_SURFACE ( (
 ( 1.000000000000000000, 0.9876883405951377704, 1.000000000000000000, 0.9876883405951377704, 1.000000000000000000, 0.9876883405951377704, 1.000000000000000000, 0.9876883405951377704, 1.000000000000000000, 0.9876883405951377704, 1.000000000000000000, 0.9876883405951377704, 1.000000000000000000, 0.9876883405951377704, 1.000000000000000000, 0.9876883405951377704, 1.000000000000000000),
 ( 1.000000000000000000, 0.9876883405951377704, 1.000000000000000000, 0.9876883405951377704, 1.000000000000000000, 0.9876883405951377704, 1.000000000000000000, 0.9876883405951377704, 1.000000000000000000, 0.9876883405951377704, 1.000000000000000000, 0.9876883405951377704, 1.000000000000000000, 0.9876883405951377704, 1.000000000000000000, 0.9876883405951377704, 1.000000000000000000) ) ) 
 REPRESENTATION_ITEM ( '' )  SURFACE ( )  );
#12550 = VERTEX_POINT ( 'NONE', #11200 ) ;
#12551 = EDGE_CURVE ( 'NONE', #9421, #8597, #12406, .T. ) ;
#12552 = DIRECTION ( 'NONE',  ( 0.000000000000000000, 0.000000000000000000, 1.000000000000000000 ) ) ;
#12553 = DIRECTION ( 'NONE',  ( 1.000000000000000000, 0.000000000000000000, 0.000000000000000000 ) ) ;
#12554 = ORIENTED_EDGE ( 'NONE', *, *, #14086, .T. ) ;
#12555 = CIRCLE ( 'NONE', #6450, 4.400000000000000355 ) ;
#12556 = DIRECTION ( 'NONE',  ( 1.000000000000000000, 0.000000000000000000, 0.000000000000000000 ) ) ;
#12557 = DIRECTION ( 'NONE',  ( 1.000000000000000000, 0.000000000000000000, 0.000000000000000000 ) ) ;
#12558 = CIRCLE ( 'NONE', #14101, 4.400000000000000355 ) ;
#12559 = ORIENTED_EDGE ( 'NONE', *, *, #4418, .F. ) ;
#12560 = CARTESIAN_POINT ( 'NONE',  ( 0.000000000000000000, 0.000000000000000000, 0.000000000000000000 ) ) ;
#12561 = VERTEX_POINT ( 'NONE', #13195 ) ;
#12562 = AXIS2_PLACEMENT_3D ( 'NONE', #9755, #9856, #17543 ) ;
#12563 = APPLICATION_PROTOCOL_DEFINITION ( 'draft international standard', 'automotive_design', 1998, #884 ) ;
#12564 = CARTESIAN_POINT ( 'NONE',  ( -5.575441324182703440, -1.185096637661177343, -12.00000000000000533 ) ) ;
#12565 = ADVANCED_FACE ( 'NONE', ( #3594 ), #12903, .F. ) ;
#12566 = AXIS2_PLACEMENT_3D ( 'NONE', #1869, #17276, #18382 ) ;
#12567 = ORIENTED_EDGE ( 'NONE', *, *, #16075, .F. ) ;
#12568 = ORIENTED_EDGE ( 'NONE', *, *, #18519, .T. ) ;
#12569 = CARTESIAN_POINT ( 'NONE',  ( 0.5279273746168616777, 26.57710921259767645, -4.996265754456091557 ) ) ;
#12570 = CARTESIAN_POINT ( 'NONE',  ( 2.789999999999999147, -9.836394144775550075, -22.71065055754462492 ) ) ;
#12571 = VERTEX_POINT ( 'NONE', #13002 ) ;
#12572 = EDGE_CURVE ( 'NONE', #13180, #5891, #549, .T. ) ;
#12573 = CARTESIAN_POINT ( 'NONE',  ( 2.030753616560879493, 24.80264696524883306, 12.05220173035447750 ) ) ;
#12574 = ORIENTED_EDGE ( 'NONE', *, *, #1468, .T. ) ;
#12575 = CIRCLE ( 'NONE', #8054, 6.000000000000021316 ) ;
#12576 = AXIS2_PLACEMENT_3D ( 'NONE', #8790, #16296, #2572 ) ;
#12577 = CARTESIAN_POINT ( 'NONE',  ( -4.484949146646406426, -3.631840208645763735, -10.50000000000000533 ) ) ;
#12578 = DIRECTION ( 'NONE',  ( -1.000000000000000000, -0.000000000000000000, -0.000000000000000000 ) ) ;
#12579 = DIRECTION ( 'NONE',  ( 1.000000000000000000, 0.000000000000000000, 0.000000000000000000 ) ) ;
#12580 = VERTEX_POINT ( 'NONE', #14300 ) ;
#12581 = CARTESIAN_POINT ( 'NONE',  ( 7.937500000000000000, 4.582717761692664205, -0.7089489049740167470 ) ) ;
#12582 = ADVANCED_FACE ( 'NONE', ( #15802 ), #6971, .F. ) ;
#12583 = ORIENTED_EDGE ( 'NONE', *, *, #2688, .T. ) ;
#12584 = ORIENTED_EDGE ( 'NONE', *, *, #5299, .F. ) ;
#12585 = CARTESIAN_POINT ( 'NONE',  ( 2.765633920072238627, 5.391175441198956086, -24.15498966839956907 ) ) ;
#12586 = CARTESIAN_POINT ( 'NONE',  ( -15.00000000000000355, 0.000000000000000000, 0.000000000000000000 ) ) ;
#12587 = CARTESIAN_POINT ( 'NONE',  ( 17.28688694438834972, -7.664027248171309203, 32.00000000000000000 ) ) ;
#12588 = CARTESIAN_POINT ( 'NONE',  ( 2.620002426024544029, 5.142044285764750811, -12.50000000000000533 ) ) ;
#12589 = ORIENTED_EDGE ( 'NONE', *, *, #16372, .F. ) ;
#12590 = FACE_OUTER_BOUND ( 'NONE', #7187, .T. ) ;
#12591 = DIRECTION ( 'NONE',  ( -1.000000000000000000, -0.000000000000000000, -0.000000000000000000 ) ) ;
#12592 =( GEOMETRIC_REPRESENTATION_CONTEXT ( 3 ) GLOBAL_UNCERTAINTY_ASSIGNED_CONTEXT ( ( #802 ) ) GLOBAL_UNIT_ASSIGNED_CONTEXT ( ( #13780, #8982, #16888 ) ) REPRESENTATION_CONTEXT ( 'NONE', 'WORKASPACE' ) );
#12593 = AXIS2_PLACEMENT_3D ( 'NONE', #6771, #17399, #9807 ) ;
#12594 = ORIENTED_EDGE ( 'NONE', *, *, #1125, .F. ) ;
#12595 = CARTESIAN_POINT ( 'NONE',  ( -90.00000000000000000, 0.000000000000000000, -6.735000000000022524 ) ) ;
#12596 = ADVANCED_FACE ( 'NONE', ( #11399 ), #2090, .T. ) ;
#12597 = ADVANCED_FACE ( 'NONE', ( #6778 ), #601, .F. ) ;
#12598 = EDGE_CURVE ( 'NONE', #736, #9247, #11305, .T. ) ;
#12599 = CARTESIAN_POINT ( 'NONE',  ( 8.843749997951615427, -4.861323657744403448, -0.5109457054262123155 ) ) ;
#12600 = CIRCLE ( 'NONE', #13548, 1.000000000000000888 ) ;
#12601 = CARTESIAN_POINT ( 'NONE',  ( 13.00000000000000000, 4.125339889944109828, -2.622041954598519187 ) ) ;
#12602 = CARTESIAN_POINT ( 'NONE',  ( -1.906188514513426096E-16, -24.22479935914659066, -2.133490293297270579 ) ) ;
#12603 = CARTESIAN_POINT ( 'NONE',  ( 2.873153789725797491, -3.954556930911881985, -9.468749997951615427 ) ) ;
#12604 = VERTEX_POINT ( 'NONE', #11497 ) ;
#12605 = DIRECTION ( 'NONE',  ( 1.000000000000000000, 0.000000000000000000, 0.000000000000000000 ) ) ;
#12606 = CARTESIAN_POINT ( 'NONE',  ( 17.11901729331276556, 5.562305898749055011, 32.00000000000000000 ) ) ;
#12607 = EDGE_CURVE ( 'NONE', #4727, #22, #18467, .T. ) ;
#12608 = CARTESIAN_POINT ( 'NONE',  ( -7.671566133830872047, 15.77352024078954429, 32.00000000000000000 ) ) ;
#12609 = ORIENTED_EDGE ( 'NONE', *, *, #10628, .T. ) ;
#12610 = CARTESIAN_POINT ( 'NONE',  ( 7.812499995903224637, 5.387740456496234565, -2.068159791354183596 ) ) ;
#12611 = VECTOR ( 'NONE', #45, 1000.000000000000000 ) ;
#12612 = PLANE ( 'NONE',  #1390 ) ;
#12613 = CARTESIAN_POINT ( 'NONE',  ( 11.96874999795161365, 1.773574444220725299, 4.620319390059829168 ) ) ;
#12614 = DIRECTION ( 'NONE',  ( 0.000000000000000000, 0.000000000000000000, -1.000000000000000000 ) ) ;
#12615 = ORIENTED_EDGE ( 'NONE', *, *, #8331, .F. ) ;
#12616 = CARTESIAN_POINT ( 'NONE',  ( 0.006974657972265005043, 23.92335783895637746, 5.408388659524176134 ) ) ;
#12617 = CYLINDRICAL_SURFACE ( 'NONE', #897, 5.700000000000001954 ) ;
#12618 = ORIENTED_EDGE ( 'NONE', *, *, #13365, .F. ) ;
#12619 = CARTESIAN_POINT ( 'NONE',  ( 14.34374999795161365, -3.499494075959791672, -3.499494075959840078 ) ) ;
#12620 = FACE_OUTER_BOUND ( 'NONE', #16662, .T. ) ;
#12621 = VERTEX_POINT ( 'NONE', #2771 ) ;
#12622 = PRODUCT_DEFINITION ( 'UNKNOWN', '', #12440, #1388 ) ;
#12623 = AXIS2_PLACEMENT_3D ( 'NONE', #6320, #12348, #15352 ) ;
#12624 = CARTESIAN_POINT ( 'NONE',  ( 13.00000000000000178, 3.789407127742559833, -3.087705756618140285 ) ) ;
#12625 = CARTESIAN_POINT ( 'NONE',  ( 9.812499995903225525, 4.080749450109650844, -4.080749450109650844 ) ) ;
#12626 = EDGE_LOOP ( 'NONE', ( #12942, #9451, #18655, #1945 ) ) ;
#12627 = DIRECTION ( 'NONE',  ( -1.000000000000000000, -0.000000000000000000, -0.000000000000000000 ) ) ;
#12628 = CARTESIAN_POINT ( 'NONE',  ( 1.039999999999999369, -12.52377138324206918, -25.12109765559666741 ) ) ;
#12629 = EDGE_CURVE ( 'NONE', #12630, #14571, #6954, .T. ) ;
#12630 = VERTEX_POINT ( 'NONE', #7567 ) ;
#12631 = DIRECTION ( 'NONE',  ( 0.000000000000000000, 0.000000000000000000, 1.000000000000000000 ) ) ;
#12632 = EDGE_LOOP ( 'NONE', ( #18071, #1394, #10846, #3858 ) ) ;
#12633 = EDGE_CURVE ( 'NONE', #3138, #13831, #5874, .T. ) ;
#12634 = DIRECTION ( 'NONE',  ( 1.000000000000000000, 0.000000000000000000, 0.000000000000000000 ) ) ;
#12635 = EDGE_LOOP ( 'NONE', ( #8064, #6797, #12282, #12527 ) ) ;
#12636 = CARTESIAN_POINT ( 'NONE',  ( 2.765633920072238183, 2.336989772644269436, 24.63872515616083447 ) ) ;
#12637 = DIRECTION ( 'NONE',  ( -1.000000000000000000, 0.000000000000000000, -0.000000000000000000 ) ) ;
#12638 = DIRECTION ( 'NONE',  ( 0.000000000000000000, -1.000000000000000000, 0.000000000000000000 ) ) ;
#12639 = AXIS2_PLACEMENT_3D ( 'NONE', #14500, #12989, #19082 ) ;
#12640 = CARTESIAN_POINT ( 'NONE',  ( 3.846120219227923798, -3.114526743279282250, -11.96874999795161365 ) ) ;
#12641 = AXIS2_PLACEMENT_3D ( 'NONE', #12178, #13878, #68 ) ;
#12642 = ORIENTED_EDGE ( 'NONE', *, *, #3261, .T. ) ;
#12643 = CARTESIAN_POINT ( 'NONE',  ( 0.6102186610125081012, 23.94322454545469370, 12.96989951879415770 ) ) ;
#12644 = ADVANCED_FACE ( 'NONE', ( #14988 ), #1385, .F. ) ;
#12645 = CARTESIAN_POINT ( 'NONE',  ( 2.790000000000000924, 0.000000000000000000, 0.000000000000000000 ) ) ;
#12646 = EDGE_LOOP ( 'NONE', ( #3167, #17649 ) ) ;
#12647 = CARTESIAN_POINT ( 'NONE',  ( -3.954556930911881096, -2.873153789725797935, -14.46874999795161720 ) ) ;
#12648 = ADVANCED_FACE ( 'NONE', ( #1183 ), #18194, .F. ) ;
#12649 = CARTESIAN_POINT ( 'NONE',  ( -10.58013454126452224, -14.56230589874905235, -35.00000000000000000 ) ) ;
#12650 = CARTESIAN_POINT ( 'NONE',  ( 2.789999999999999147, 22.25075486061751207, -9.324097380959219805 ) ) ;
#12651 = ORIENTED_EDGE ( 'NONE', *, *, #18251, .F. ) ;
#12652 = CIRCLE ( 'NONE', #15206, 9.000000000000019540 ) ;
#12653 = CARTESIAN_POINT ( 'NONE',  ( 8.000000000000005329, -5.668774803599153422, -0.5958122406256771697 ) ) ;
#12654 = CARTESIAN_POINT ( 'NONE',  ( 11.31249999590322375, 1.185096637661293251, -5.575441324182679459 ) ) ;
#12655 = VECTOR ( 'NONE', #11235, 1000.000000000000000 ) ;
#12656 = ORIENTED_EDGE ( 'NONE', *, *, #2168, .F. ) ;
#12657 = PLANE ( 'NONE',  #12920 ) ;
#12658 = ORIENTED_EDGE ( 'NONE', *, *, #914, .T. ) ;
#12659 = APPLICATION_PROTOCOL_DEFINITION ( 'draft international standard', 'automotive_design', 1998, #4709 ) ;
#12660 = CARTESIAN_POINT ( 'NONE',  ( -5.209999999999999964, 0.000000000000000000, 0.000000000000000000 ) ) ;
#12661 = CARTESIAN_POINT ( 'NONE',  ( 9.343749997951615427, 4.780397808154257078, 1.280903732194454303 ) ) ;
#12662 = EDGE_LOOP ( 'NONE', ( #3427, #10442, #2914, #11140, #12113, #3029, #4835 ) ) ;
#12663 = ORIENTED_EDGE ( 'NONE', *, *, #18962, .F. ) ;
#12664 = CARTESIAN_POINT ( 'NONE',  ( -19.00000000000000355, 1.224646799147353207E-16, 0.000000000000000000 ) ) ;
#12665 = CARTESIAN_POINT ( 'NONE',  ( 0.000000000000000000, 0.000000000000000000, -18.00000000000000355 ) ) ;
#12666 = ORIENTED_EDGE ( 'NONE', *, *, #2486, .T. ) ;
#12667 = EDGE_CURVE ( 'NONE', #9386, #3914, #12719, .T. ) ;
#12668 =( BOUNDED_CURVE ( )  B_SPLINE_CURVE ( 2, ( #11242, #14246, #6718, #9551, #3635, #4838, #14143, #15847, #5233, #3343, #17346, #5128, #15749, #9758, #18842, #8338, #6618 ),
 .UNSPECIFIED., .F., .F. ) 
 B_SPLINE_CURVE_WITH_KNOTS ( ( 3, 2, 2, 2, 2, 2, 2, 2, 3 ),
 ( 0.000000000000000000, 0.05000000000000000971, 0.1000000000000000194, 0.1499999999999999944, 0.2000000000000000389, 0.2500000000000000000, 0.2999999999999999889, 0.3499999999999999223, 0.4000000000000000777 ),
 .UNSPECIFIED. ) 
 CURVE ( )  GEOMETRIC_REPRESENTATION_ITEM ( )  RATIONAL_B_SPLINE_CURVE ( ( 1.000000000000000000, 0.9876883405951377704, 1.000000000000000000, 0.9876883405951377704, 1.000000000000000000, 0.9876883405951377704, 1.000000000000000000, 0.9876883405951377704, 1.000000000000000000, 0.9876883405951377704, 1.000000000000000000, 0.9876883405951377704, 1.000000000000000000, 0.9876883405951377704, 1.000000000000000000, 0.9876883405951377704, 1.000000000000000000 ) ) 
 REPRESENTATION_ITEM ( '' )  );
#12669 = VECTOR ( 'NONE', #721, 1000.000000000000000 ) ;
#12670 = CIRCLE ( 'NONE', #4036, 9.000000000000001776 ) ;
#12671 =( NAMED_UNIT ( * ) PLANE_ANGLE_UNIT ( ) SI_UNIT ( $, .RADIAN. ) );
#12672 = ORIENTED_EDGE ( 'NONE', *, *, #18017, .F. ) ;
#12673 = DIRECTION ( 'NONE',  ( 1.000000000000000000, 0.000000000000000000, -0.000000000000000000 ) ) ;
#12674 = LINE ( 'NONE', #4866, #8716 ) ;
#12675 = FACE_BOUND ( 'NONE', #8165, .T. ) ;
#12676 = ORIENTED_EDGE ( 'NONE', *, *, #12165, .T. ) ;
#12678 = CARTESIAN_POINT ( 'NONE',  ( 13.00000000000000000, -0.2080849974988778772, -4.883670121236158401 ) ) ;
#12677 = B_SPLINE_CURVE_WITH_KNOTS ( 'NONE', 3,
 ( #14574, #10265, #1054, #7133 ),
 .UNSPECIFIED., .F., .F.,
 ( 4, 4 ),
 ( 0.005258110598983630792, 0.005948376585272738271 ),
 .UNSPECIFIED. ) ;
#12679 = CARTESIAN_POINT ( 'NONE',  ( 2.789999999999999147, 0.000000000000000000, 0.000000000000000000 ) ) ;
#12680 = CIRCLE ( 'NONE', #6903, 4.000000000000000000 ) ;
#12681 = EDGE_LOOP ( 'NONE', ( #19466, #12221, #19382, #6139, #8152, #9961, #166, #6549, #579 ) ) ;
#12682 = ORIENTED_EDGE ( 'NONE', *, *, #11125, .F. ) ;
#12683 = CARTESIAN_POINT ( 'NONE',  ( -4.233219804643852946, 2.444050593750049405, -11.46874999795161543 ) ) ;
#12684 = CARTESIAN_POINT ( 'NONE',  ( 13.00000000000000000, 4.125339889944109828, -2.622041954598519187 ) ) ;
#12685 = CARTESIAN_POINT ( 'NONE',  ( -3.632567103900569361, -3.270778111535287191, -7.843749997951614539 ) ) ;
#12686 = VERTEX_POINT ( 'NONE', #15187 ) ;
#12687 = CARTESIAN_POINT ( 'NONE',  ( 10.84374999795161543, 1.016293382781477961, -4.781284448697179279 ) ) ;
#12688 = DIRECTION ( 'NONE',  ( 0.000000000000000000, 0.000000000000000000, 1.000000000000000000 ) ) ;
#12689 = VECTOR ( 'NONE', #1083, 1000.000000000000000 ) ;
#12690 = VERTEX_POINT ( 'NONE', #1482 ) ;
#12691 = DIRECTION ( 'NONE',  ( 0.000000000000000000, 0.7806247497997995666, 0.6250000000000002220 ) ) ;
#12692 = ADVANCED_FACE ( 'NONE', ( #15089 ), #4477, .F. ) ;
#12693 = LINE ( 'NONE', #12402, #17918 ) ;
#12694 = CARTESIAN_POINT ( 'NONE',  ( -41.99999999999999289, 4.999999999999998224, -2.000000000000000000 ) ) ;
#12695 = CARTESIAN_POINT ( 'NONE',  ( -8.671566133830875600, 15.77352024078954429, -35.00000000000000000 ) ) ;
#12696 = AXIS2_PLACEMENT_3D ( 'NONE', #3416, #9625, #12819 ) ;
#12697 = CARTESIAN_POINT ( 'NONE',  ( 8.343749997951613651, 4.942249507334556924, -0.2590123213420975623 ) ) ;
#12698 = ORIENTED_EDGE ( 'NONE', *, *, #4560, .F. ) ;
#12699 = CYLINDRICAL_SURFACE ( 'NONE', #10125, 28.06981291497571362 ) ;
#12700 = CARTESIAN_POINT ( 'NONE',  ( 1.039999999999997593, 0.000000000000000000, 0.000000000000000000 ) ) ;
#12701 = DIRECTION ( 'NONE',  ( -1.000000000000000000, -0.000000000000000000, 0.000000000000000000 ) ) ;
#12702 = ORIENTED_EDGE ( 'NONE', *, *, #16030, .F. ) ;
#12703 = DIRECTION ( 'NONE',  ( 0.000000000000000000, 0.000000000000000000, -1.000000000000000000 ) ) ;
#12704 = AXIS2_PLACEMENT_3D ( 'NONE', #18924, #11429, #5316 ) ;
#12705 = SURFACE_SIDE_STYLE ('',( #18898 ) ) ;
#12706 = CARTESIAN_POINT ( 'NONE',  ( 9.468749997951615427, 4.465502636338023912, 1.988169868018593300 ) ) ;
#12707 = LINE ( 'NONE', #12415, #14612 ) ;
#12708 = DIRECTION ( 'NONE',  ( 0.000000000000000000, 0.000000000000000000, 1.000000000000000000 ) ) ;
#12709 = EDGE_CURVE ( 'NONE', #8648, #1328, #16233, .T. ) ;
#12710 = VERTEX_POINT ( 'NONE', #7466 ) ;
#12711 = DIRECTION ( 'NONE',  ( -1.000000000000000000, 0.000000000000000000, 0.000000000000000000 ) ) ;
#12712 = CARTESIAN_POINT ( 'NONE',  ( 2.780931166827226519, -21.10834851580694504, -12.54305517365643929 ) ) ;
#12713 = ORIENTED_EDGE ( 'NONE', *, *, #4521, .T. ) ;
#12714 = CARTESIAN_POINT ( 'NONE',  ( 8.312499995903225525, -1.761396867937238486, 5.421022142882364392 ) ) ;
#12715 = B_SPLINE_CURVE_WITH_KNOTS ( 'NONE', 3,
 ( #3924, #6909, #8621, #14638, #16034, #11342 ),
 .UNSPECIFIED., .F., .F.,
 ( 4, 2, 4 ),
 ( 4.462636695652347161E-07, 0.001879885036799764601, 0.003759323809929963987 ),
 .UNSPECIFIED. ) ;
#12716 = CARTESIAN_POINT ( 'NONE',  ( -5.207209108562804722, 2.318398865532109276, -14.00000000000000533 ) ) ;
#12717 = ORIENTED_EDGE ( 'NONE', *, *, #8490, .T. ) ;
#12718 = EDGE_CURVE ( 'NONE', #1853, #2859, #4089, .T. ) ;
#12719 = CIRCLE ( 'NONE', #894, 22.00000000000000355 ) ;
#12720 = AXIS2_PLACEMENT_3D ( 'NONE', #13617, #13814, #18031 ) ;
#12721 = CARTESIAN_POINT ( 'NONE',  ( 2.444050593749960587, -4.233219804643904460, -6.656249997951614539 ) ) ;
#12722 = CYLINDRICAL_SURFACE ( 'NONE', #14509, 1.000000000000002665 ) ;
#12723 = ORIENTED_EDGE ( 'NONE', *, *, #5992, .T. ) ;
#12724 = CARTESIAN_POINT ( 'NONE',  ( 0.02436607992776498519, 9.836394144775706394, 22.71065055754456097 ) ) ;
#12725 = PRESENTATION_STYLE_ASSIGNMENT (( #7640 ) ) ;
#12726 = CARTESIAN_POINT ( 'NONE',  ( 2.299999999999996270, 0.000000000000000000, -9.000000000000021316 ) ) ;
#12727 = ORIENTED_EDGE ( 'NONE', *, *, #8389, .F. ) ;
#12728 = CARTESIAN_POINT ( 'NONE',  ( 7.968749997951616315, -2.246813503491864150, 4.409619785863891472 ) ) ;
#12729 = ORIENTED_EDGE ( 'NONE', *, *, #18615, .F. ) ;
#12730 = CARTESIAN_POINT ( 'NONE',  ( 2.765633920072242624, -22.71065055754459650, 9.836394144775621129 ) ) ;
#12731 = ORIENTED_EDGE ( 'NONE', *, *, #1951, .T. ) ;
#12732 = PLANE ( 'NONE',  #4148 ) ;
#12733 = DIRECTION ( 'NONE',  ( 0.000000000000000000, 0.000000000000000000, 1.000000000000000000 ) ) ;
#12734 = EDGE_CURVE ( 'NONE', #12395, #7772, #4731, .T. ) ;
#12735 = PRODUCT_DEFINITION_SHAPE ( 'NONE', 'NONE',  #19701 ) ;
#12736 = CARTESIAN_POINT ( 'NONE',  ( 2.257825477245773982, 18.57583492944447556, -19.66801664102683489 ) ) ;
#12737 = AXIS2_PLACEMENT_3D ( 'NONE', #3566, #8172, #5268 ) ;
#12738 = CARTESIAN_POINT ( 'NONE',  ( 0.7589665203264061022, 19.86422722021312026, 19.12621924769873161 ) ) ;
#12739 = ORIENTED_EDGE ( 'NONE', *, *, #14959, .T. ) ;
#12740 = FACE_BOUND ( 'NONE', #8078, .T. ) ;
#12741 = DIRECTION ( 'NONE',  ( 1.000000000000000000, 0.000000000000000000, 0.000000000000000000 ) ) ;
#12742 = EDGE_CURVE ( 'NONE', #9816, #15555, #4382, .T. ) ;
#12743 = ORIENTED_EDGE ( 'NONE', *, *, #6666, .F. ) ;
#12744 = EDGE_CURVE ( 'NONE', #8623, #12225, #5987, .T. ) ;
#12745 = CARTESIAN_POINT ( 'NONE',  ( -6.626241948324210540, -16.73597674598852336, -32.00000000000000000 ) ) ;
#12746 = DIRECTION ( 'NONE',  ( 0.000000000000000000, 0.000000000000000000, 1.000000000000000000 ) ) ;
#12747 = DIRECTION ( 'NONE',  ( -1.000000000000000000, 0.000000000000000000, 0.000000000000000000 ) ) ;
#12748 = EDGE_LOOP ( 'NONE', ( #11623, #3572, #655, #2871 ) ) ;
#12749 = CARTESIAN_POINT ( 'NONE',  ( 7.626241948324204323, -16.73597674598852691, -35.00000000000000000 ) ) ;
#12750 = DIRECTION ( 'NONE',  ( -1.000000000000000000, -0.000000000000000000, -0.000000000000000000 ) ) ;
#12751 = CARTESIAN_POINT ( 'NONE',  ( 9.843749997951615427, 0.5109457054261445919, 4.861323657744411442 ) ) ;
#12752 = ORIENTED_EDGE ( 'NONE', *, *, #19364, .T. ) ;
#12753 = EDGE_CURVE ( 'NONE', #3618, #7112, #13686, .T. ) ;
#12754 = FACE_OUTER_BOUND ( 'NONE', #12488, .T. ) ;
#12755 = ORIENTED_EDGE ( 'NONE', *, *, #14677, .F. ) ;
#12756 = CARTESIAN_POINT ( 'NONE',  ( 9.843749997951615427, 0.5109457054261445919, 4.861323657744411442 ) ) ;
#12757 = PRODUCT_DEFINITION_FORMATION_WITH_SPECIFIED_SOURCE ( 'ANY', '', #17533, .NOT_KNOWN. ) ;
#12758 = CARTESIAN_POINT ( 'NONE',  ( 11.34374999795161543, 3.114526743279255161, 3.846120219227944670 ) ) ;
#12759 = VERTEX_POINT ( 'NONE', #7258 ) ;
#12760 = VERTEX_POINT ( 'NONE', #5575 ) ;
#12761 = DIRECTION ( 'NONE',  ( -1.000000000000000000, -0.000000000000000000, -0.000000000000000000 ) ) ;
#12762 = CARTESIAN_POINT ( 'NONE',  ( -2.299999999999996270, 0.000000000000000000, 0.000000000000000000 ) ) ;
#12763 = CARTESIAN_POINT ( 'NONE',  ( 7.468749997951615427, 3.270778111535313837, 3.632567103900546712 ) ) ;
#12764 = EDGE_CURVE ( 'NONE', #10294, #17165, #1218, .T. ) ;
#12765 = VERTEX_POINT ( 'NONE', #2571 ) ;
#12766 = AXIS2_PLACEMENT_3D ( 'NONE', #19255, #11756, #18966 ) ;
#12767 = FILL_AREA_STYLE_COLOUR ( '', #13820 ) ;
#12768 = VERTEX_POINT ( 'NONE', #11789 ) ;
#12769 = EDGE_CURVE ( 'NONE', #13000, #9369, #17516, .T. ) ;
#12770 = CARTESIAN_POINT ( 'NONE',  ( 11.50000000000000355, 2.068159791354183596, 5.387740456496233676 ) ) ;
#12771 = CARTESIAN_POINT ( 'NONE',  ( 0.3020334839682081163, -5.763142191869158992, -7.500000000000005329 ) ) ;
#12772 = EDGE_CURVE ( 'NONE', #12027, #5242, #2672, .T. ) ;
#12773 = FACE_OUTER_BOUND ( 'NONE', #16860, .T. ) ;
#12774 = PLANE ( 'NONE',  #139 ) ;
#12775 = ORIENTED_EDGE ( 'NONE', *, *, #6616, .T. ) ;
#12776 = FACE_OUTER_BOUND ( 'NONE', #14364, .T. ) ;
#12777 =( NAMED_UNIT ( * ) PLANE_ANGLE_UNIT ( ) SI_UNIT ( $, .RADIAN. ) );
#12778 = CARTESIAN_POINT ( 'NONE',  ( -2.000000000000001776, 0.000000000000000000, 0.000000000000000000 ) ) ;
#12779 = VERTEX_POINT ( 'NONE', #13383 ) ;
#12780 = ORIENTED_EDGE ( 'NONE', *, *, #18271, .T. ) ;
#12781 = CARTESIAN_POINT ( 'NONE',  ( -4.942249507334553371, 0.2590123213421660631, -9.968749997951617203 ) ) ;
#12782 = AXIS2_PLACEMENT_3D ( 'NONE', #430, #1731, #12436 ) ;
#12783 = CARTESIAN_POINT ( 'NONE',  ( 13.00000000000000000, 4.091807895435353615, -2.674798881044243792 ) ) ;
#12784 = CARTESIAN_POINT ( 'NONE',  ( 0.7592463965288823724, -12.98165646470099155, 24.32906614999610895 ) ) ;
#12785 = VERTEX_POINT ( 'NONE', #5768 ) ;
#12786 = CARTESIAN_POINT ( 'NONE',  ( -2.500000000000001776, 0.000000000000000000, -6.200000000000020606 ) ) ;
#12787 = CARTESIAN_POINT ( 'NONE',  ( 12.34374999795161543, -4.888101187499994893, -0.7741991708319226895 ) ) ;
#12788 = B_SPLINE_CURVE_WITH_KNOTS ( 'NONE', 3,
 ( #11094, #16909, #12497, #14000 ),
 .UNSPECIFIED., .F., .F.,
 ( 4, 4 ),
 ( 1.981826382900849143E-07, 0.0006887856082032019125 ),
 .UNSPECIFIED. ) ;
#12789 = VERTEX_POINT ( 'NONE', #11885 ) ;
#12790 = DIRECTION ( 'NONE',  ( -0.000000000000000000, -1.000000000000000000, -0.000000000000000000 ) ) ;
#12791 = CARTESIAN_POINT ( 'NONE',  ( 6.000000000000005329, 0.000000000000000000, -5.700000000000001066 ) ) ;
#12792 = AXIS2_PLACEMENT_3D ( 'NONE', #3378, #10691, #13785 ) ;
#12793 = AXIS2_PLACEMENT_3D ( 'NONE', #6210, #4924, #14027 ) ;
#12794 = EDGE_CURVE ( 'NONE', #8320, #13895, #8436, .T. ) ;
#12795 = CARTESIAN_POINT ( 'NONE',  ( -5.700000000000001066, -0.2987243419133009947, -10.47794484381773650 ) ) ;
#12796 = DIRECTION ( 'NONE',  ( 1.000000000000000000, 0.000000000000000000, 0.000000000000000000 ) ) ;
#12797 = CARTESIAN_POINT ( 'NONE',  ( 4.409619785863891472, -2.246813503491864150, -7.968749997951616315 ) ) ;
#12798 = DIRECTION ( 'NONE',  ( 0.000000000000000000, 0.000000000000000000, -1.000000000000000000 ) ) ;
#12799 = VERTEX_POINT ( 'NONE', #18678 ) ;
#12800 = DIRECTION ( 'NONE',  ( 0.000000000000000000, 0.000000000000000000, -1.000000000000000000 ) ) ;
#12801 = FILL_AREA_STYLE ('',( #11201 ) ) ;
#12802 = CARTESIAN_POINT ( 'NONE',  ( 17.96448111170888851, 1.130229351527639148, -32.00000000000000000 ) ) ;
#12803 = EDGE_CURVE ( 'NONE', #16376, #10624, #17724, .T. ) ;
#12804 = CARTESIAN_POINT ( 'NONE',  ( 13.96874999795161365, -4.780397808154265960, 1.280903732194421663 ) ) ;
#12805 = CARTESIAN_POINT ( 'NONE',  ( -1.000000000000001998, 18.00000000000000355, 35.00000000000000000 ) ) ;
#12806 = VERTEX_POINT ( 'NONE', #15488 ) ;
#12807 = FACE_OUTER_BOUND ( 'NONE', #4989, .T. ) ;
#12808 = VECTOR ( 'NONE', #9593, 1000.000000000000000 ) ;
#12809 = CARTESIAN_POINT ( 'NONE',  ( -18.11901729331277267, 5.562305898749051458, -32.00000000000000000 ) ) ;
#12810 = CIRCLE ( 'NONE', #3852, 2.524999999999996803 ) ;
#12811 = ORIENTED_EDGE ( 'NONE', *, *, #51, .T. ) ;
#12812 = DIRECTION ( 'NONE',  ( 1.000000000000000000, 0.000000000000000000, 0.000000000000000000 ) ) ;
#12813 = CARTESIAN_POINT ( 'NONE',  ( 0.000000000000000000, 2.680914349914567470E-13, -23.06981291497571362 ) ) ;
#12814 = ORIENTED_EDGE ( 'NONE', *, *, #19472, .F. ) ;
#12815 = CARTESIAN_POINT ( 'NONE',  ( -1.899999999999999023, 1.010590785124388747E-15, 8.239200000000002078 ) ) ;
#12816 = EDGE_CURVE ( 'NONE', #15252, #9066, #3129, .T. ) ;
#12817 = CYLINDRICAL_SURFACE ( 'NONE', #11533, 13.19999999999999929 ) ;
#12818 = DIRECTION ( 'NONE',  ( 0.000000000000000000, 0.000000000000000000, 1.000000000000000000 ) ) ;
#12819 = DIRECTION ( 'NONE',  ( 0.000000000000000000, 0.000000000000000000, 1.000000000000000000 ) ) ;
#12820 = VERTEX_POINT ( 'NONE', #1774 ) ;
#12821 = VECTOR ( 'NONE', #3035, 1000.000000000000000 ) ;
#12822 = FACE_OUTER_BOUND ( 'NONE', #13885, .T. ) ;
#12823 = FACE_OUTER_BOUND ( 'NONE', #13448, .T. ) ;
#12824 = ORIENTED_EDGE ( 'NONE', *, *, #16644, .T. ) ;
#12825 = FACE_OUTER_BOUND ( 'NONE', #14511, .T. ) ;
#12826 = ORIENTED_EDGE ( 'NONE', *, *, #8714, .F. ) ;
#12827 = CYLINDRICAL_SURFACE ( 'NONE', #3436, 1.000000000000000888 ) ;
#12828 = VERTEX_POINT ( 'NONE', #12290 ) ;
#12829 = CARTESIAN_POINT ( 'NONE',  ( 0.1882238946918232125, -2.857713464478510268, -25.78859396478530996 ) ) ;
#12830 = EDGE_CURVE ( 'NONE', #10514, #11541, #5674, .T. ) ;
#12831 = DIRECTION ( 'NONE',  ( 0.000000000000000000, 0.000000000000000000, 1.000000000000000000 ) ) ;
#12832 = DIRECTION ( 'NONE',  ( 1.000000000000000000, 0.000000000000000000, 0.000000000000000000 ) ) ;
#12833 = CARTESIAN_POINT ( 'NONE',  ( 4.465502636338039011, 1.988169868018562436, -8.843749997951615427 ) ) ;
#12834 = ORIENTED_EDGE ( 'NONE', *, *, #17955, .T. ) ;
#12835 = FACE_OUTER_BOUND ( 'NONE', #17191, .T. ) ;
#12836 = DIRECTION ( 'NONE',  ( 1.000000000000000000, 0.000000000000000000, 0.000000000000000000 ) ) ;
#12837 = VECTOR ( 'NONE', #17027, 999.9999999999998863 ) ;
#12838 = ORIENTED_EDGE ( 'NONE', *, *, #19266, .T. ) ;
#12839 = AXIS2_PLACEMENT_3D ( 'NONE', #7347, #2861, #13573 ) ;
#12840 = FACE_OUTER_BOUND ( 'NONE', #17843, .T. ) ;
#12841 = CARTESIAN_POINT ( 'NONE',  ( -15.00000000000000355, 1.224646799147353454E-16, 0.000000000000000000 ) ) ;
#12842 = EDGE_CURVE ( 'NONE', #1726, #18935, #12234, .T. ) ;
#12843 = FACE_OUTER_BOUND ( 'NONE', #9265, .T. ) ;
#12844 = EDGE_CURVE ( 'NONE', #12070, #13382, #1679, .T. ) ;
#12845 = VERTEX_POINT ( 'NONE', #12481 ) ;
#12846 = CARTESIAN_POINT ( 'NONE',  ( 1.039999999999996261, 24.89775460606850999, -12.96210679857759018 ) ) ;
#12847 = FACE_BOUND ( 'NONE', #1595, .T. ) ;
#12848 = CARTESIAN_POINT ( 'NONE',  ( 13.00000000000000178, -0.3952618871915391519, -4.872094134945741395 ) ) ;
#12849 = ORIENTED_EDGE ( 'NONE', *, *, #1846, .F. ) ;
#12850 = CARTESIAN_POINT ( 'NONE',  ( 0.02436607992775978102, 16.37294372382885044, -18.55949924794875017 ) ) ;
#12851 = EDGE_CURVE ( 'NONE', #12571, #17039, #3142, .T. ) ;
#12852 = AXIS2_PLACEMENT_3D ( 'NONE', #14598, #8491, #7056 ) ;
#12853 = VERTEX_POINT ( 'NONE', #4874 ) ;
#12854 = CIRCLE ( 'NONE', #16055, 3.000000000000000000 ) ;
#12855 = CARTESIAN_POINT ( 'NONE',  ( 8.343749997951611874, 2.695436003842704764, 4.150607464521812062 ) ) ;
#12856 = CARTESIAN_POINT ( 'NONE',  ( 11.96874999795161365, 1.773574444220725299, 4.620319390059829168 ) ) ;
#12857 = AXIS2_PLACEMENT_3D ( 'NONE', #15516, #9118, #4708 ) ;
#12858 = VERTEX_POINT ( 'NONE', #16989 ) ;
#12859 = ORIENTED_EDGE ( 'NONE', *, *, #4890, .T. ) ;
#12860 = CARTESIAN_POINT ( 'NONE',  ( 4.648860486681943627, -1.510506337161893864, -7.843749997951614539 ) ) ;
#12861 = CARTESIAN_POINT ( 'NONE',  ( 10.96874999795161720, -1.773574444220757496, 4.620319390059819398 ) ) ;
#12862 = ORIENTED_EDGE ( 'NONE', *, *, #11726, .T. ) ;
#12863 = CARTESIAN_POINT ( 'NONE',  ( -4.465502636338051445, -1.988169868018530462, -8.843749997951615427 ) ) ;
#12864 = CIRCLE ( 'NONE', #19562, 4.500000000000000000 ) ;
#12865 = ORIENTED_EDGE ( 'NONE', *, *, #4682, .T. ) ;
#12866 = AXIS2_PLACEMENT_3D ( 'NONE', #7853, #9271, #7448 ) ;
#12867 = VECTOR ( 'NONE', #11794, 1000.000000000000000 ) ;
#12868 = CARTESIAN_POINT ( 'NONE',  ( 13.00000000000000533, -0.5958122406256377568, 5.668774803599156975 ) ) ;
#12869 = AXIS2_PLACEMENT_3D ( 'NONE', #13071, #11662, #14580 ) ;
#12870 = CARTESIAN_POINT ( 'NONE',  ( 10.50000000000000533, -5.700000000000006395, 0.9027913098498173694 ) ) ;
#12871 = CARTESIAN_POINT ( 'NONE',  ( -8.776855558857221240, 3.635492607468361115, 12.00000000000000000 ) ) ;
#12872 = ORIENTED_EDGE ( 'NONE', *, *, #1272, .T. ) ;
#12873 = DIRECTION ( 'NONE',  ( 1.000000000000000000, 1.776356839400250465E-15, 0.000000000000000000 ) ) ;
#12874 = DIRECTION ( 'NONE',  ( 0.000000000000000000, 0.000000000000000000, 1.000000000000000000 ) ) ;
#12875 = SURFACE_SIDE_STYLE ('',( #17768 ) ) ;
#12876 = EDGE_CURVE ( 'NONE', #10239, #14216, #15293, .T. ) ;
#12877 = ORIENTED_EDGE ( 'NONE', *, *, #15473, .T. ) ;
#12878 = EDGE_LOOP ( 'NONE', ( #18659, #10966, #6448, #13459 ) ) ;
#12879 = EDGE_CURVE ( 'NONE', #13120, #307, #9553, .T. ) ;
#12880 = CARTESIAN_POINT ( 'NONE',  ( -0.5958122406255597081, 5.668774803599165857, -14.00000000000000533 ) ) ;
#12881 = VECTOR ( 'NONE', #8654, 1000.000000000000000 ) ;
#12882 = CARTESIAN_POINT ( 'NONE',  ( 2.789999999999999147, -15.04425356660744839, -20.70663861606288236 ) ) ;
#12883 = CYLINDRICAL_SURFACE ( 'NONE', #8174, 1.000000000000004441 ) ;
#12884 = ORIENTED_EDGE ( 'NONE', *, *, #18367, .F. ) ;
#12885 = ADVANCED_FACE ( 'NONE', ( #8065 ), #12387, .T. ) ;
#12886 = CARTESIAN_POINT ( 'NONE',  ( 9.468749997951615427, -0.5109457054261099529, -4.861323657744413218 ) ) ;
#12887 = CARTESIAN_POINT ( 'NONE',  ( 12.84374999795161543, 3.632567103900569361, -3.270778111535288080 ) ) ;
#12888 = EDGE_LOOP ( 'NONE', ( #6777, #17122 ) ) ;
#12889 = CARTESIAN_POINT ( 'NONE',  ( 1.869199999999999973, 0.000000000000000000, -8.239200000000002078 ) ) ;
#12890 = CARTESIAN_POINT ( 'NONE',  ( 8.000000000000005329, 3.350375938067097437, -4.611396867937201272 ) ) ;
#12891 = COLOUR_RGB ( '', 0.08235294, 0.09019608, 0.10196078) ;
#12892 = EDGE_CURVE ( 'NONE', #5362, #15740, #16523, .T. ) ;
#12893 = CARTESIAN_POINT ( 'NONE',  ( 0.7589665203264086557, -19.86422722021297815, -19.12621924769889148 ) ) ;
#12894 = CARTESIAN_POINT ( 'NONE',  ( 7.289885936478948558, 4.956617915597515633, -0.4930775504667603837 ) ) ;
#12895 = CARTESIAN_POINT ( 'NONE',  ( 3.954556930911842016, -2.873153789725853002, -8.468749997951615427 ) ) ;
#12896 = PRODUCT ( 'machine screw nut hex_ai_MSHXNUT 0.375-16-S-N', 'machine screw nut hex_ai_MSHXNUT 0.375-16-S-N', '', ( #15365 ) ) ;
#12897 = CARTESIAN_POINT ( 'NONE',  ( 8.671566133830875600, 15.77352024078954784, 35.00000000000000000 ) ) ;
#12898 =( NAMED_UNIT ( * ) PLANE_ANGLE_UNIT ( ) SI_UNIT ( $, .RADIAN. ) );
#12899 = LINE ( 'NONE', #14695, #8695 ) ;
#12900 = AXIS2_PLACEMENT_3D ( 'NONE', #6892, #9830, #14713 ) ;
#12901 = CARTESIAN_POINT ( 'NONE',  ( -2.000000000000001776, 8.247996192257451316E-16, 6.735000000000022524 ) ) ;
#12902 = EDGE_LOOP ( 'NONE', ( #17430, #10733 ) ) ;
#12903 = CYLINDRICAL_SURFACE ( 'NONE', #19109, 8.265000000000021885 ) ;
#12904 = CARTESIAN_POINT ( 'NONE',  ( -18.11901729331277267, 5.562305898749051458, -35.00000000000000000 ) ) ;
#12905 = CARTESIAN_POINT ( 'NONE',  ( 5.000000000000000000, 1.999999999999998224, 37.99999999999999289 ) ) ;
#12906 = CARTESIAN_POINT ( 'NONE',  ( 10.84374999795161543, -3.632567103900500971, -3.270778111535363131 ) ) ;
#12907 = DIRECTION ( 'NONE',  ( 0.000000000000000000, -1.000000000000000000, 0.000000000000000000 ) ) ;
#12908 = CARTESIAN_POINT ( 'NONE',  ( 2.718184767880469810, -10.24584646439555691, 23.19431517146929878 ) ) ;
#12909 = ORIENTED_EDGE ( 'NONE', *, *, #5716, .T. ) ;
#12910 = CARTESIAN_POINT ( 'NONE',  ( 10.50000000000000533, 2.068159791354258648, -5.387740456496205255 ) ) ;
#12911 = ADVANCED_FACE ( 'NONE', ( #12184 ), #7962, .F. ) ;
#12912 = CARTESIAN_POINT ( 'NONE',  ( 2.000000000000001776, 0.000000000000000000, 0.000000000000000000 ) ) ;
#12913 = ORIENTED_EDGE ( 'NONE', *, *, #2669, .F. ) ;
#12914 = DIRECTION ( 'NONE',  ( -1.000000000000000000, -0.000000000000000000, -0.000000000000000000 ) ) ;
#12915 = CARTESIAN_POINT ( 'NONE',  ( 9.000000000000001776, 0.000000000000000000, -22.00000000000000000 ) ) ;
#12916 = ADVANCED_FACE ( 'NONE', ( #16893 ), #3174, .F. ) ;
#12917 = CARTESIAN_POINT ( 'NONE',  ( 2.789999999999999147, -18.28042085475289369, 15.74360496233375173 ) ) ;
#12918 = CARTESIAN_POINT ( 'NONE',  ( 0.8944271909999177428, 0.000000000000000000, 0.000000000000000000 ) ) ;
#12919 = VERTEX_POINT ( 'NONE', #13886 ) ;
#12920 = AXIS2_PLACEMENT_3D ( 'NONE', #9358, #1750, #149 ) ;
#12921 = FACE_OUTER_BOUND ( 'NONE', #15943, .T. ) ;
#12922 = CARTESIAN_POINT ( 'NONE',  ( -3.143139765844555900, 4.840010801796527318, -13.81249999590322730 ) ) ;
#12923 = CARTESIAN_POINT ( 'NONE',  ( 1.869199999999999973, 0.000000000000000000, 0.000000000000000000 ) ) ;
#12924 = ORIENTED_EDGE ( 'NONE', *, *, #3409, .F. ) ;
#12925 = CARTESIAN_POINT ( 'NONE',  ( 8.968749997951611874, -3.499494075959840966, 3.499494075959791672 ) ) ;
#12926 = ORIENTED_EDGE ( 'NONE', *, *, #17245, .T. ) ;
#12927 = LINE ( 'NONE', #19025, #13037 ) ;
#12928 = EDGE_LOOP ( 'NONE', ( #13969, #18203, #10915, #17348 ) ) ;
#12929 = B_SPLINE_CURVE_WITH_KNOTS ( 'NONE', 3,
 ( #12917, #13019, #4103, #2586 ),
 .UNSPECIFIED., .F., .F.,
 ( 4, 4 ),
 ( 0.005258110598983608240, 0.005948376585272733934 ),
 .UNSPECIFIED. ) ;
#12930 = EDGE_CURVE ( 'NONE', #3019, #12710, #178, .T. ) ;
#12931 = B_SPLINE_CURVE_WITH_KNOTS ( 'NONE', 1,
 ( #5092, #6579 ),
 .UNSPECIFIED., .F., .F.,
 ( 2, 2 ),
 ( 0.000000000000000000, 1.000000000000000000 ),
 .UNSPECIFIED. ) ;
#12932 = FACE_OUTER_BOUND ( 'NONE', #16582, .T. ) ;
#12933 = CIRCLE ( 'NONE', #7479, 1.000000000000000888 ) ;
#12934 = CARTESIAN_POINT ( 'NONE',  ( -30.00000000000000000, 4.200000000000000178, 5.143516556418882928E-16 ) ) ;
#12935 = CARTESIAN_POINT ( 'NONE',  ( -9.000000000000000000, 1.102182119232617714E-15, 35.00000000000000000 ) ) ;
#12936 = CARTESIAN_POINT ( 'NONE',  ( -5.142044285764751699, 2.620002426024544029, -7.500000000000005329 ) ) ;
#12937 = EDGE_LOOP ( 'NONE', ( #17499, #15768, #5559, #19145 ) ) ;
#12938 = CARTESIAN_POINT ( 'NONE',  ( 0.000000000000000000, 0.000000000000000000, 32.00000000000000000 ) ) ;
#12939 = EDGE_CURVE ( 'NONE', #8859, #18804, #16577, .T. ) ;
#12940 = DIRECTION ( 'NONE',  ( -1.000000000000000000, 0.000000000000000000, 0.000000000000000000 ) ) ;
#12941 = CIRCLE ( 'NONE', #7163, 4.400000000000000355 ) ;
#12942 = ORIENTED_EDGE ( 'NONE', *, *, #15494, .F. ) ;
#12943 = DIRECTION ( 'NONE',  ( 0.000000000000000000, 0.000000000000000000, 1.000000000000000000 ) ) ;
#12944 = EDGE_CURVE ( 'NONE', #6633, #1107, #13687, .T. ) ;
#12945 = AXIS2_PLACEMENT_3D ( 'NONE', #4796, #3397, #200 ) ;
#12946 = CYLINDRICAL_SURFACE ( 'NONE', #12188, 1.000000000000002887 ) ;
#12947 = CARTESIAN_POINT ( 'NONE',  ( 2.783068888626321513, 22.53293026234517171, -9.685942809246819607 ) ) ;
#12948 = ORIENTED_EDGE ( 'NONE', *, *, #8652, .T. ) ;
#12949 = CYLINDRICAL_SURFACE ( 'NONE', #2360, 0.9999999999999974465 ) ;
#12950 = CARTESIAN_POINT ( 'NONE',  ( -3.383411828340740850E-14, -4.888101187500000222, -11.46874999795161543 ) ) ;
#12951 = DIRECTION ( 'NONE',  ( 0.000000000000000000, 0.000000000000000000, -1.000000000000000000 ) ) ;
#12952 = VERTEX_POINT ( 'NONE', #6755 ) ;
#12953 = CARTESIAN_POINT ( 'NONE',  ( 1.039999999999996705, -27.68468304288255410, -4.633866840649218055 ) ) ;
#12954 = CIRCLE ( 'NONE', #17103, 9.000000000000001776 ) ;
#12955 = ORIENTED_EDGE ( 'NONE', *, *, #1391, .F. ) ;
#12956 = DIRECTION ( 'NONE',  ( 0.000000000000000000, -1.000000000000000000, 0.000000000000000000 ) ) ;
#12957 = DIRECTION ( 'NONE',  ( -0.000000000000000000, -0.000000000000000000, 1.000000000000000000 ) ) ;
#12958 = CARTESIAN_POINT ( 'NONE',  ( -5.209999999999999964, 0.000000000000000000, 0.000000000000000000 ) ) ;
#12959 = ORIENTED_EDGE ( 'NONE', *, *, #8076, .F. ) ;
#12960 =( BOUNDED_CURVE ( )  B_SPLINE_CURVE ( 2, ( #8563, #9979, #14672, #10464, #4258, #10562, #4453, #3045, #16568, #19453, #16660, #17968, #12062, #1253, #12161 ),
 .UNSPECIFIED., .F., .F. ) 
 B_SPLINE_CURVE_WITH_KNOTS ( ( 3, 2, 2, 2, 2, 2, 2, 3 ),
 ( 0.000000000000000000, 0.05000000000000000971, 0.1000000000000000194, 0.1499999999999999944, 0.2000000000000000389, 0.2500000000000000000, 0.2999999999999999889, 0.3265529187307102399 ),
 .UNSPECIFIED. ) 
 CURVE ( )  GEOMETRIC_REPRESENTATION_ITEM ( )  RATIONAL_B_SPLINE_CURVE ( ( 1.000000000000000000, 0.9876883405951377704, 1.000000000000000000, 0.9876883405951377704, 1.000000000000000000, 0.9876883405951377704, 1.000000000000000000, 0.9876883405951377704, 1.000000000000000000, 0.9876883405951377704, 1.000000000000000000, 0.9876883405951377704, 1.000000000000000000, 0.9934617901676501273, 0.9938679225082089896 ) ) 
 REPRESENTATION_ITEM ( '' )  );
#12961 = ORIENTED_EDGE ( 'NONE', *, *, #8157, .T. ) ;
#12962 = CARTESIAN_POINT ( 'NONE',  ( 4.888101187499994893, -0.7741991708319229115, -7.343749997951615427 ) ) ;
#12963 = CARTESIAN_POINT ( 'NONE',  ( -17.68117051311639898, -3.372863662543042818, 35.00000000000000000 ) ) ;
#12964 = DIRECTION ( 'NONE',  ( 0.000000000000000000, 0.000000000000000000, 1.000000000000000000 ) ) ;
#12965 = EDGE_LOOP ( 'NONE', ( #4611, #15808, #10, #347 ) ) ;
#12966 = EDGE_CURVE ( 'NONE', #16866, #10948, #19168, .T. ) ;
#12967 = CIRCLE ( 'NONE', #18075, 6.000000000000000888 ) ;
#12968 = ORIENTED_EDGE ( 'NONE', *, *, #4935, .F. ) ;
#12969 = ADVANCED_FACE ( 'NONE', ( #778 ), #8860, .T. ) ;
#12970 = AXIS2_PLACEMENT_3D ( 'NONE', #4562, #1466, #7446 ) ;
#12971 = CARTESIAN_POINT ( 'NONE',  ( -2.444050593749990785, 4.233219804643887585, -6.843749997951615427 ) ) ;
#12972 = CARTESIAN_POINT ( 'NONE',  ( 2.789999999999999147, -22.25075486061744812, 9.324097380959361914 ) ) ;
#12973 = DIRECTION ( 'NONE',  ( 1.000000000000000000, 0.000000000000000000, 0.000000000000000000 ) ) ;
#12974 = FILL_AREA_STYLE ('',( #10171 ) ) ;
#12975 = CARTESIAN_POINT ( 'NONE',  ( 0.5109457054261784537, 4.861323657744407001, -8.468749997951615427 ) ) ;
#12976 = VERTEX_POINT ( 'NONE', #2366 ) ;
#12977 = ORIENTED_EDGE ( 'NONE', *, *, #18387, .T. ) ;
#12978 = DIRECTION ( 'NONE',  ( 1.000000000000000000, 0.000000000000000000, 0.000000000000000000 ) ) ;
#12979 = VECTOR ( 'NONE', #13629, 1000.000000000000000 ) ;
#12980 = AXIS2_PLACEMENT_3D ( 'NONE', #8002, #15915, #3607 ) ;
#12981 = EDGE_CURVE ( 'NONE', #1526, #1723, #9891, .T. ) ;
#12982 = CARTESIAN_POINT ( 'NONE',  ( -19.00000000000000355, -4.215373648918917304, 3.375000000000000888 ) ) ;
#12983 = PRODUCT_DEFINITION ( 'UNKNOWN', '', #7626, #5968 ) ;
#12984 = CARTESIAN_POINT ( 'NONE',  ( -12.32184790671639085, 13.12143529358541549, -32.00000000000000000 ) ) ;
#12985 = ORIENTED_EDGE ( 'NONE', *, *, #3458, .T. ) ;
#12986 = CARTESIAN_POINT ( 'NONE',  ( 6.468749997951615427, -4.233219804643852946, -2.444050593750049849 ) ) ;
#12987 = CARTESIAN_POINT ( 'NONE',  ( 13.00000000000000000, -4.125339889944092953, 2.622041954598548941 ) ) ;
#12988 = ORIENTED_EDGE ( 'NONE', *, *, #19319, .F. ) ;
#12989 = DIRECTION ( 'NONE',  ( -0.000000000000000000, -0.000000000000000000, 1.000000000000000000 ) ) ;
#12990 = EDGE_CURVE ( 'NONE', #11367, #12173, #16047, .T. ) ;
#12991 = VECTOR ( 'NONE', #18597, 1000.000000000000114 ) ;
#12992 = AXIS2_PLACEMENT_3D ( 'NONE', #1586, #9099, #14900 ) ;
#12993 = CARTESIAN_POINT ( 'NONE',  ( 0.000000000000000000, 0.000000000000000000, 29.00000000000000355 ) ) ;
#12994 = CARTESIAN_POINT ( 'NONE',  ( 2.789999999999999147, 24.44424927289184879, 0.2301004812061933913 ) ) ;
#12995 = CARTESIAN_POINT ( 'NONE',  ( 12.84374999795161543, 1.016293382781411792, 4.781284448697195266 ) ) ;
#12996 = DIRECTION ( 'NONE',  ( 0.000000000000000000, 0.000000000000000000, 1.000000000000000000 ) ) ;
#12997 =( NAMED_UNIT ( * ) PLANE_ANGLE_UNIT ( ) SI_UNIT ( $, .RADIAN. ) );
#12998 = CARTESIAN_POINT ( 'NONE',  ( 111.3234999999999957, 0.000000000000000000, 0.000000000000000000 ) ) ;
#12999 = CARTESIAN_POINT ( 'NONE',  ( 2.765633920072238627, -21.30679549418621832, -12.59161484032935618 ) ) ;
#13000 = VERTEX_POINT ( 'NONE', #15978 ) ;
#13001 = EDGE_CURVE ( 'NONE', #3237, #18640, #18976, .T. ) ;
#13002 = CARTESIAN_POINT ( 'NONE',  ( -36.00000000000000000, -2.000000000000000888, 5.000000000000000000 ) ) ;
#13003 = FACE_OUTER_BOUND ( 'NONE', #18354, .T. ) ;
#13004 = UNCERTAINTY_MEASURE_WITH_UNIT (LENGTH_MEASURE( 1.000000000000000082E-05 ), #294, 'distance_accuracy_value', 'NONE');
#13005 = CARTESIAN_POINT ( 'NONE',  ( 4.484949146646356688, -3.631840208645826351, -12.81249999590322552 ) ) ;
#13006 = CARTESIAN_POINT ( 'NONE',  ( 9.468749997951615427, -4.465502636338009701, -1.988169868018624609 ) ) ;
#13007 = CYLINDRICAL_SURFACE ( 'NONE', #737, 28.06981291497571362 ) ;
#13008 = TOROIDAL_SURFACE ( 'NONE', #13322, -32.79058411375427795, 40.00000000000000711 ) ;
#13009 = CARTESIAN_POINT ( 'NONE',  ( 2.765633920072235519, -9.836394144775869819, 22.71065055754449347 ) ) ;
#13010 = EDGE_CURVE ( 'NONE', #14916, #9647, #19433, .T. ) ;
#13011 = VECTOR ( 'NONE', #18317, 1000.000000000000000 ) ;
#13012 = VERTEX_POINT ( 'NONE', #14280 ) ;
#13013 = DIRECTION ( 'NONE',  ( 0.000000000000000000, 0.000000000000000000, 1.000000000000000000 ) ) ;
#13014 = TOROIDAL_SURFACE ( 'NONE', #10782, 24.12539914357697413, 8.000000000000000000 ) ;
#13015 = DIRECTION ( 'NONE',  ( 0.000000000000000000, -1.000000000000000000, 0.000000000000000000 ) ) ;
#13016 = ORIENTED_EDGE ( 'NONE', *, *, #1052, .T. ) ;
#13017 = CARTESIAN_POINT ( 'NONE',  ( -22.00000000000000355, 2.694222958124177204E-15, 32.00000000000000000 ) ) ;
#13018 = CARTESIAN_POINT ( 'NONE',  ( -2.000000000000000000, 7.174999999999999822, 0.000000000000000000 ) ) ;
#13019 = CARTESIAN_POINT ( 'NONE',  ( 2.790000000000000480, -18.34424029220122776, 15.96500990068118497 ) ) ;
#13020 = CARTESIAN_POINT ( 'NONE',  ( -11.00000000000000355, -3.278623949159159778, 2.625000000000000888 ) ) ;
#13021 = ORIENTED_EDGE ( 'NONE', *, *, #15653, .F. ) ;
#13022 = AXIS2_PLACEMENT_3D ( 'NONE', #6805, #13222, #4110 ) ;
#13023 = DIRECTION ( 'NONE',  ( 1.000000000000000000, 0.000000000000000000, 0.000000000000000000 ) ) ;
#13024 = CARTESIAN_POINT ( 'NONE',  ( 2.030753610301984313, -19.86438386685646762, -19.12676442129367516 ) ) ;
#13025 = ORIENTED_EDGE ( 'NONE', *, *, #14735, .T. ) ;
#13026 = DIRECTION ( 'NONE',  ( 1.000000000000000000, 0.000000000000000000, 0.000000000000000000 ) ) ;
#13027 = EDGE_LOOP ( 'NONE', ( #7329, #2315 ) ) ;
#13028 = CARTESIAN_POINT ( 'NONE',  ( 8.812499995903225525, -5.763142191869158992, 0.3020334839682081163 ) ) ;
#13029 = ORIENTED_EDGE ( 'NONE', *, *, #443, .T. ) ;
#13030 = CARTESIAN_POINT ( 'NONE',  ( -3.631935042553950055, 7.068536848887553958, 4.616894251167434456E-15 ) ) ;
#13031 = CARTESIAN_POINT ( 'NONE',  ( 0.5279273746168626769, -4.996265754456183927, -26.57710921259766224 ) ) ;
#13032 = DIRECTION ( 'NONE',  ( -1.000000000000000000, 0.000000000000000000, -0.000000000000000000 ) ) ;
#13033 = CARTESIAN_POINT ( 'NONE',  ( 0.02436607992775934733, -2.336989772644440855, 24.63872515616082026 ) ) ;
#13034 = ORIENTED_EDGE ( 'NONE', *, *, #8974, .F. ) ;
#13035 = FACE_BOUND ( 'NONE', #4994, .T. ) ;
#13036 = DIRECTION ( 'NONE',  ( 0.000000000000000000, 0.000000000000000000, -1.000000000000000000 ) ) ;
#13037 = VECTOR ( 'NONE', #9938, 1000.000000000000000 ) ;
#13038 = ORIENTED_EDGE ( 'NONE', *, *, #15653, .T. ) ;
#13039 = AXIS2_PLACEMENT_3D ( 'NONE', #14211, #405, #2003 ) ;
#13040 = LINE ( 'NONE', #5521, #1334 ) ;
#13041 = CARTESIAN_POINT ( 'NONE',  ( 5.699999596629369059, -0.002144393866035136480, -6.000593838912648081 ) ) ;
#13042 = ORIENTED_EDGE ( 'NONE', *, *, #10069, .F. ) ;
#13043 = LINE ( 'NONE', #16046, #11991 ) ;
#13044 = CARTESIAN_POINT ( 'NONE',  ( 4.611396867937178179, -3.350375938067129855, -8.000000000000005329 ) ) ;
#13045 = FACE_BOUND ( 'NONE', #15287, .T. ) ;
#13046 = ORIENTED_EDGE ( 'NONE', *, *, #615, .F. ) ;
#13047 = CARTESIAN_POINT ( 'NONE',  ( 2.789999999999999147, 23.48180575137737947, -5.535312321042476391 ) ) ;
#13048 = AXIS2_PLACEMENT_3D ( 'NONE', #5385, #5187, #14404 ) ;
#13049 = VERTEX_POINT ( 'NONE', #17381 ) ;
#13050 = ITEM_DEFINED_TRANSFORMATION ( 'NONE', 'NONE', #8923,  #16724 ) ;
#13051 = DIRECTION ( 'NONE',  ( 6.419766481290786633E-33, -1.000000000000000000, 0.000000000000000000 ) ) ;
#13052 = VECTOR ( 'NONE', #17897, 1000.000000000000000 ) ;
#13053 = DIRECTION ( 'NONE',  ( 1.000000000000000000, 0.000000000000000000, 0.000000000000000000 ) ) ;
#13054 = LINE ( 'NONE', #1040, #7708 ) ;
#13055 = ORIENTED_EDGE ( 'NONE', *, *, #15258, .F. ) ;
#13056 = CARTESIAN_POINT ( 'NONE',  ( 0.7188676524878460095, -24.19190980169966210, 12.96989951879399428 ) ) ;
#13057 = FACE_OUTER_BOUND ( 'NONE', #11248, .T. ) ;
#13058 = DIRECTION ( 'NONE',  ( 0.000000000000000000, 0.6818181818181816567, -0.7315216790650493905 ) ) ;
#13059 = EDGE_CURVE ( 'NONE', #15888, #16011, #6967, .T. ) ;
#13060 = ORIENTED_EDGE ( 'NONE', *, *, #15430, .T. ) ;
#13061 = CARTESIAN_POINT ( 'NONE',  ( 2.765633920072234631, 16.37294372382885044, -18.55949924794875017 ) ) ;
#13062 = PRODUCT ( 'double end studs bm=1.5d_am_AM A M8X100-N', 'double end studs bm=1.5d_am_AM A M8X100-N', '', ( #5045 ) ) ;
#13063 = CIRCLE ( 'NONE', #15937, 1.000000000000002665 ) ;
#13064 = ORIENTED_EDGE ( 'NONE', *, *, #1325, .F. ) ;
#13065 = CARTESIAN_POINT ( 'NONE',  ( 12.99999999999998757, -0.02830770314431023046, 5.175540411820490405 ) ) ;
#13066 = AXIS2_PLACEMENT_3D ( 'NONE', #2263, #2361, #8473 ) ;
#13067 = CARTESIAN_POINT ( 'NONE',  ( -2.500000000000002220, 0.000000000000000000, 0.000000000000000000 ) ) ;
#13068 = VERTEX_POINT ( 'NONE', #10376 ) ;
#13069 =( BOUNDED_SURFACE ( )  B_SPLINE_SURFACE ( 1, 2, ( 
 ( #15211, #16313, #7181, #10414, #19404, #5691, #16513, #11807, #8905, #15009, #1300, #7379, #7791, #7587, #9408, #10802, #6281 ),
 ( #10707, #16912, #4698, #4990, #7687, #1596, #15407, #6374, #11097, #3191, #16818, #14092, #3092, #17200, #13904, #9603, #6184 ) ),
 .UNSPECIFIED., .F., .F., .F. ) 
 B_SPLINE_SURFACE_WITH_KNOTS ( ( 2, 2 ),
 ( 3, 2, 2, 2, 2, 2, 2, 2, 3 ),
 ( 0.000000000000000000, 1.000000000000000000 ),
 ( 0.000000000000000000, 0.05000000000000000278, 0.1000000000000000056, 0.1499999999999999944, 0.2000000000000000111, 0.2500000000000000000, 0.2999999999999999889, 0.3499999999999999778, 0.4000000000000000222 ),
 .UNSPECIFIED. ) 
 GEOMETRIC_REPRESENTATION_ITEM ( )  RATIONAL_B_SPLINE_SURFACE ( (
 ( 1.000000000000000000, 0.9876883405951377704, 1.000000000000000000, 0.9876883405951377704, 1.000000000000000000, 0.9876883405951377704, 1.000000000000000000, 0.9876883405951377704, 1.000000000000000000, 0.9876883405951377704, 1.000000000000000000, 0.9876883405951377704, 1.000000000000000000, 0.9876883405951377704, 1.000000000000000000, 0.9876883405951377704, 1.000000000000000000),
 ( 1.000000000000000000, 0.9876883405951377704, 1.000000000000000000, 0.9876883405951377704, 1.000000000000000000, 0.9876883405951377704, 1.000000000000000000, 0.9876883405951377704, 1.000000000000000000, 0.9876883405951377704, 1.000000000000000000, 0.9876883405951377704, 1.000000000000000000, 0.9876883405951377704, 1.000000000000000000, 0.9876883405951377704, 1.000000000000000000) ) ) 
 REPRESENTATION_ITEM ( '' )  SURFACE ( )  );
#13070 = CARTESIAN_POINT ( 'NONE',  ( -2.255998204157477538, -17.85806462366060288, 35.00000000000000000 ) ) ;
#13071 = CARTESIAN_POINT ( 'NONE',  ( 2.789999999999999147, 14.18181402625742749, 19.91106274590519121 ) ) ;
#13072 = ORIENTED_EDGE ( 'NONE', *, *, #15007, .T. ) ;
#13073 = ORIENTED_EDGE ( 'NONE', *, *, #1414, .F. ) ;
#13074 = DIRECTION ( 'NONE',  ( 0.000000000000000000, 0.000000000000000000, 1.000000000000000000 ) ) ;
#13075 = CIRCLE ( 'NONE', #18494, 24.12539914357697768 ) ;
#13076 = EDGE_CURVE ( 'NONE', #126, #411, #7338, .T. ) ;
#13077 = CARTESIAN_POINT ( 'NONE',  ( 2.262072706628476926, -18.56460150496924655, -19.66369668717053898 ) ) ;
#13078 = DIRECTION ( 'NONE',  ( -0.000000000000000000, -0.000000000000000000, 1.000000000000000000 ) ) ;
#13079 = ORIENTED_EDGE ( 'NONE', *, *, #3722, .F. ) ;
#13080 = DIRECTION ( 'NONE',  ( 0.000000000000000000, 0.000000000000000000, 1.000000000000000000 ) ) ;
#13081 = CARTESIAN_POINT ( 'NONE',  ( 11.84374999795161365, 2.444050593750049405, -4.233219804643852946 ) ) ;
#13082 = VERTEX_POINT ( 'NONE', #5851 ) ;
#13083 = PLANE ( 'NONE',  #5908 ) ;
#13084 = CARTESIAN_POINT ( 'NONE',  ( 2.765633920072241736, -9.836394144775550075, -22.71065055754462492 ) ) ;
#13085 = CARTESIAN_POINT ( 'NONE',  ( -1.800000000000000044, 9.552245033349356544E-16, 7.800000000000000711 ) ) ;
#13086 = ADVANCED_FACE ( 'NONE', ( #13270 ), #2651, .F. ) ;
#13087 = CARTESIAN_POINT ( 'NONE',  ( 0.000000000000000000, 0.000000000000000000, -5.946610266546040968 ) ) ;
#13088 = EDGE_CURVE ( 'NONE', #5753, #11765, #13063, .T. ) ;
#13089 = STYLED_ITEM ( 'NONE', ( #13664 ), #16042 ) ;
#13090 = DIRECTION ( 'NONE',  ( 1.000000000000000000, -0.000000000000000000, -0.000000000000000000 ) ) ;
#13091 =( LENGTH_UNIT ( ) NAMED_UNIT ( * ) SI_UNIT ( .MILLI., .METRE. ) );
#13092 = CARTESIAN_POINT ( 'NONE',  ( 2.788130827028544534, 20.90869469097885158, -12.51925356660739297 ) ) ;
#13093 = ORIENTED_EDGE ( 'NONE', *, *, #2521, .F. ) ;
#13094 = CARTESIAN_POINT ( 'NONE',  ( -10.58013454126452224, -14.56230589874905235, 32.00000000000000000 ) ) ;
#13095 = EDGE_CURVE ( 'NONE', #12361, #14452, #17535, .T. ) ;
#13096 = PLANE ( 'NONE',  #12576 ) ;
#13097 = CARTESIAN_POINT ( 'NONE',  ( 4.620319390059819398, -1.773574444220757274, -11.34374999795161543 ) ) ;
#13098 = EDGE_CURVE ( 'NONE', #569, #3340, #10175, .T. ) ;
#13099 = CARTESIAN_POINT ( 'NONE',  ( 2.783025228907522131, -9.686319561461109728, 22.53337530003400246 ) ) ;
#13100 = CARTESIAN_POINT ( 'NONE',  ( 1.016293382781377819, -4.781284448697200595, -7.843749997951614539 ) ) ;
#13101 = ORIENTED_EDGE ( 'NONE', *, *, #9015, .T. ) ;
#13102 = DIRECTION ( 'NONE',  ( 0.000000000000000000, 0.000000000000000000, -1.000000000000000000 ) ) ;
#13103 = DIRECTION ( 'NONE',  ( 0.000000000000000000, 0.000000000000000000, 1.000000000000000000 ) ) ;
#13104 = AXIS2_PLACEMENT_3D ( 'NONE', #11032, #6312, #9744 ) ;
#13105 = ORIENTED_EDGE ( 'NONE', *, *, #6311, .T. ) ;
#13106 = DIRECTION ( 'NONE',  ( 0.000000000000000000, 0.000000000000000000, -1.000000000000000000 ) ) ;
#13107 = AXIS2_PLACEMENT_3D ( 'NONE', #8611, #14628, #2312 ) ;
#13108 = ADVANCED_FACE ( 'NONE', ( #11864 ), #11966, .F. ) ;
#13109 = DIRECTION ( 'NONE',  ( -0.000000000000000000, -0.000000000000000000, 1.000000000000000000 ) ) ;
#13110 = DIRECTION ( 'NONE',  ( 0.4999999999999978351, -0.8660254037844398178, 0.000000000000000000 ) ) ;
#13111 = DIRECTION ( 'NONE',  ( -0.000000000000000000, -0.000000000000000000, 1.000000000000000000 ) ) ;
#13112 = ORIENTED_EDGE ( 'NONE', *, *, #3006, .T. ) ;
#13113 = CARTESIAN_POINT ( 'NONE',  ( 2.789999999999999147, -24.34211360614294506, -7.909232158575071558 ) ) ;
#13114 = SURFACE_SIDE_STYLE ('',( #14529 ) ) ;
#13115 = EDGE_CURVE ( 'NONE', #7654, #1041, #10507, .T. ) ;
#13116 = CARTESIAN_POINT ( 'NONE',  ( 0.000000000000000000, 0.000000000000000000, 29.00000000000000355 ) ) ;
#13117 = CARTESIAN_POINT ( 'NONE',  ( 2.789999999999999147, 2.680914349914567470E-13, -23.06981291497571362 ) ) ;
#13118 = ORIENTED_EDGE ( 'NONE', *, *, #8943, .F. ) ;
#13119 = CARTESIAN_POINT ( 'NONE',  ( 2.783068945535915883, -2.248820353272798389, -24.42321038836784908 ) ) ;
#13120 = VERTEX_POINT ( 'NONE', #8567 ) ;
#13121 = VECTOR ( 'NONE', #9915, 1000.000000000000000 ) ;
#13122 = CIRCLE ( 'NONE', #16954, 1.000000000000004441 ) ;
#13123 = DIRECTION ( 'NONE',  ( 0.000000000000000000, 0.000000000000000000, -1.000000000000000000 ) ) ;
#13124 = DIRECTION ( 'NONE',  ( -1.000000000000000000, 0.000000000000000000, 0.000000000000000000 ) ) ;
#13125 = EDGE_CURVE ( 'NONE', #7839, #17369, #2851, .T. ) ;
#13126 = CARTESIAN_POINT ( 'NONE',  ( 2.999999999999998224, 2.487173708821167839, -2.318181818181817899 ) ) ;
#13127 = DIRECTION ( 'NONE',  ( 0.000000000000000000, 0.000000000000000000, 1.000000000000000000 ) ) ;
#13128 = ORIENTED_EDGE ( 'NONE', *, *, #13911, .F. ) ;
#13129 = FACE_BOUND ( 'NONE', #440, .T. ) ;
#13130 = CARTESIAN_POINT ( 'NONE',  ( 16.96448111170888851, 1.130229351527639148, -35.00000000000000000 ) ) ;
#13131 = ORIENTED_EDGE ( 'NONE', *, *, #13538, .T. ) ;
#13132 = EDGE_CURVE ( 'NONE', #9713, #303, #8261, .T. ) ;
#13133 = DIRECTION ( 'NONE',  ( 0.000000000000000000, 0.000000000000000000, 1.000000000000000000 ) ) ;
#13134 = CARTESIAN_POINT ( 'NONE',  ( 4.888101187500000222, -3.413342815706642518E-14, -6.843749997951615427 ) ) ;
#13135 = EDGE_CURVE ( 'NONE', #13172, #7172, #9224, .T. ) ;
#13136 = EDGE_LOOP ( 'NONE', ( #5545, #17675 ) ) ;
#13137 = CARTESIAN_POINT ( 'NONE',  ( -20.63749999999999574, 0.000000000000000000, 0.000000000000000000 ) ) ;
#13138 = CARTESIAN_POINT ( 'NONE',  ( -2.647025296875054057, -4.584782303107560963, -6.234374998975811266 ) ) ;
#13139 = EDGE_CURVE ( 'NONE', #759, #9357, #1873, .T. ) ;
#13140 = DIRECTION ( 'NONE',  ( 1.000000000000000000, 0.000000000000000000, -0.000000000000000000 ) ) ;
#13141 = ORIENTED_EDGE ( 'NONE', *, *, #19516, .T. ) ;
#13142 = CARTESIAN_POINT ( 'NONE',  ( 0.5279272933715190019, 18.56460150496967287, -19.66369668717012331 ) ) ;
#13143 = ORIENTED_EDGE ( 'NONE', *, *, #11189, .F. ) ;
#13144 = FACE_OUTER_BOUND ( 'NONE', #14966, .T. ) ;
#13145 = FACE_OUTER_BOUND ( 'NONE', #9955, .T. ) ;
#13146 = CARTESIAN_POINT ( 'NONE',  ( 11.32184790671639263, 13.12143529358541016, -32.00000000000000000 ) ) ;
#13147 = ORIENTED_EDGE ( 'NONE', *, *, #18623, .F. ) ;
#13148 = DIRECTION ( 'NONE',  ( -1.000000000000000000, -6.419766481290786633E-33, 0.000000000000000000 ) ) ;
#13149 = CARTESIAN_POINT ( 'NONE',  ( 13.86923836996420789, -11.47363181547641453, -32.00000000000000000 ) ) ;
#13150 = CIRCLE ( 'NONE', #2591, 1.000000000000002665 ) ;
#13151 = CIRCLE ( 'NONE', #9648, 14.00000000000000178 ) ;
#13152 = DIRECTION ( 'NONE',  ( 1.000000000000000000, 0.000000000000000000, 0.000000000000000000 ) ) ;
#13153 = EDGE_LOOP ( 'NONE', ( #6239, #7405, #19332, #19610 ) ) ;
#13154 = VECTOR ( 'NONE', #8842, 1000.000000000000114 ) ;
#13155 = APPLICATION_CONTEXT ( 'automotive_design' ) ;
#13156 = FACE_OUTER_BOUND ( 'NONE', #266, .T. ) ;
#13157 = ADVANCED_FACE ( 'NONE', ( #4263 ), #1261, .F. ) ;
#13158 = ORIENTED_EDGE ( 'NONE', *, *, #11668, .F. ) ;
#13159 = EDGE_CURVE ( 'NONE', #9124, #9454, #12091, .T. ) ;
#13160 = AXIS2_PLACEMENT_3D ( 'NONE', #14832, #1126, #13236 ) ;
#13161 = AXIS2_PLACEMENT_3D ( 'NONE', #4883, #7872, #4587 ) ;
#13162 = CARTESIAN_POINT ( 'NONE',  ( -16.19790265903627713, 9.644882309621941374, -35.00000000000000000 ) ) ;
#13163 = EDGE_CURVE ( 'NONE', #19526, #17330, #16671, .T. ) ;
#13164 = AXIS2_PLACEMENT_3D ( 'NONE', #17115, #7600, #16828 ) ;
#13165 = CARTESIAN_POINT ( 'NONE',  ( 8.776855558857221240, 3.635492607468361559, 12.00000000000000000 ) ) ;
#13166 = ORIENTED_EDGE ( 'NONE', *, *, #9827, .T. ) ;
#13167 = CARTESIAN_POINT ( 'NONE',  ( -3.270778111535288080, 3.632567103900569361, -12.84374999795161543 ) ) ;
#13168 =( NAMED_UNIT ( * ) PLANE_ANGLE_UNIT ( ) SI_UNIT ( $, .RADIAN. ) );
#13169 = CARTESIAN_POINT ( 'NONE',  ( 1.988169868018593300, 4.465502636338023912, -9.468749997951615427 ) ) ;
#13170 = AXIS2_PLACEMENT_3D ( 'NONE', #10002, #19381, #3787 ) ;
#13171 = ORIENTED_EDGE ( 'NONE', *, *, #13847, .F. ) ;
#13172 = VERTEX_POINT ( 'NONE', #962 ) ;
#13173 = DIRECTION ( 'NONE',  ( 0.000000000000000000, 0.000000000000000000, 1.000000000000000000 ) ) ;
#13174 = EDGE_CURVE ( 'NONE', #7627, #6695, #14018, .T. ) ;
#13175 = CARTESIAN_POINT ( 'NONE',  ( 12.96874999795161543, -4.150607464521812062, 2.695436003842704764 ) ) ;
#13176 = ORIENTED_EDGE ( 'NONE', *, *, #5252, .F. ) ;
#13177 = VECTOR ( 'NONE', #4791, 1000.000000000000000 ) ;
#13178 = CARTESIAN_POINT ( 'NONE',  ( 0.02436607992775978102, -12.59161484032896361, -21.30679549418645280 ) ) ;
#13179 = TOROIDAL_SURFACE ( 'NONE', #7077, -21.04737509655562988, 30.00000000000000355 ) ;
#13180 = VERTEX_POINT ( 'NONE', #19360 ) ;
#13181 = AXIS2_PLACEMENT_3D ( 'NONE', #12391, #12095, #1582 ) ;
#13182 = CYLINDRICAL_SURFACE ( 'NONE', #18416, 1.000000000000000888 ) ;
#13183 = ORIENTED_EDGE ( 'NONE', *, *, #17932, .T. ) ;
#13184 = CYLINDRICAL_SURFACE ( 'NONE', #4004, 4.400000000000000355 ) ;
#13185 = AXIS2_PLACEMENT_3D ( 'NONE', #17673, #8371, #14673 ) ;
#13186 =( BOUNDED_SURFACE ( )  B_SPLINE_SURFACE ( 1, 2, ( 
 ( #11732, #19725, #10241, #10343, #2715, #5713, #15131, #12033, #18042, #7402, #8928, #15032, #4422, #13240, #5812, #6010, #16334 ),
 ( #11929, #2910, #7302, #1322, #4326, #2616, #13327, #4514, #10631, #13628, #1426, #1224, #17834, #19428, #8730, #13527, #10437 ) ),
 .UNSPECIFIED., .F., .F., .F. ) 
 B_SPLINE_SURFACE_WITH_KNOTS ( ( 2, 2 ),
 ( 3, 2, 2, 2, 2, 2, 2, 2, 3 ),
 ( 0.000000000000000000, 1.000000000000000000 ),
 ( 0.000000000000000000, 0.05000000000000000278, 0.1000000000000000056, 0.1499999999999999944, 0.2000000000000000111, 0.2500000000000000000, 0.2999999999999999889, 0.3499999999999999778, 0.4000000000000000222 ),
 .UNSPECIFIED. ) 
 GEOMETRIC_REPRESENTATION_ITEM ( )  RATIONAL_B_SPLINE_SURFACE ( (
 ( 1.000000000000000000, 0.9876883405951377704, 1.000000000000000000, 0.9876883405951377704, 1.000000000000000000, 0.9876883405951377704, 1.000000000000000000, 0.9876883405951377704, 1.000000000000000000, 0.9876883405951377704, 1.000000000000000000, 0.9876883405951377704, 1.000000000000000000, 0.9876883405951377704, 1.000000000000000000, 0.9876883405951377704, 1.000000000000000000),
 ( 1.000000000000000000, 0.9876883405951377704, 1.000000000000000000, 0.9876883405951377704, 1.000000000000000000, 0.9876883405951377704, 1.000000000000000000, 0.9876883405951377704, 1.000000000000000000, 0.9876883405951377704, 1.000000000000000000, 0.9876883405951377704, 1.000000000000000000, 0.9876883405951377704, 1.000000000000000000, 0.9876883405951377704, 1.000000000000000000) ) ) 
 REPRESENTATION_ITEM ( '' )  SURFACE ( )  );
#13187 = EDGE_CURVE ( 'NONE', #11765, #17321, #7141, .T. ) ;
#13188 = DIRECTION ( 'NONE',  ( 1.000000000000000000, -0.000000000000000000, 0.000000000000000000 ) ) ;
#13189 = DIRECTION ( 'NONE',  ( 0.000000000000000000, 1.224646799147358384E-16, 1.000000000000000000 ) ) ;
#13190 = CARTESIAN_POINT ( 'NONE',  ( 13.00000000000000178, 0.7793280607715257213, 4.825575716215943167 ) ) ;
#13191 = AXIS2_PLACEMENT_3D ( 'NONE', #15179, #10289, #19574 ) ;
#13192 = LINE ( 'NONE', #10193, #866 ) ;
#13193 = CARTESIAN_POINT ( 'NONE',  ( 2.789999999999999147, -22.71065055754445439, -9.836394144775947979 ) ) ;
#13194 = ORIENTED_EDGE ( 'NONE', *, *, #17807, .F. ) ;
#13195 = CARTESIAN_POINT ( 'NONE',  ( 1.039999999999997593, -24.89775460606841051, 12.96210679857778025 ) ) ;
#13196 = DIRECTION ( 'NONE',  ( -1.000000000000000000, -0.000000000000000000, -0.000000000000000000 ) ) ;
#13197 = UNCERTAINTY_MEASURE_WITH_UNIT (LENGTH_MEASURE( 1.000000000000000082E-05 ), #14070, 'distance_accuracy_value', 'NONE');
#13198 = DIRECTION ( 'NONE',  ( 0.000000000000000000, 1.000000000000000000, -1.224646799147353207E-16 ) ) ;
#13199 = CYLINDRICAL_SURFACE ( 'NONE', #14135, 2.524999999999995914 ) ;
#13200 = CARTESIAN_POINT ( 'NONE',  ( -5.421022142882375938, 1.761396867937200517, -8.312499995903225525 ) ) ;
#13201 = EDGE_CURVE ( 'NONE', #5854, #9684, #9138, .T. ) ;
#13202 = ORIENTED_EDGE ( 'NONE', *, *, #18978, .F. ) ;
#13203 = CYLINDRICAL_SURFACE ( 'NONE', #14114, 6.000000000000000000 ) ;
#13204 = EDGE_CURVE ( 'NONE', #12478, #17826, #7662, .T. ) ;
#13205 = EDGE_CURVE ( 'NONE', #1162, #11385, #6147, .T. ) ;
#13206 = CARTESIAN_POINT ( 'NONE',  ( -1.310841663519413114, 4.898587196589412829E-16, -4.000000000000000000 ) ) ;
#13207 = VECTOR ( 'NONE', #15157, 1000.000000000000000 ) ;
#13208 = ORIENTED_EDGE ( 'NONE', *, *, #6517, .T. ) ;
#13209 = DIRECTION ( 'NONE',  ( 0.000000000000000000, 0.000000000000000000, 1.000000000000000000 ) ) ;
#13210 = CYLINDRICAL_SURFACE ( 'NONE', #7678, 5.700000000000001954 ) ;
#13211 = EDGE_CURVE ( 'NONE', #16953, #14278, #18792, .T. ) ;
#13212 = EDGE_CURVE ( 'NONE', #4121, #14720, #18178, .T. ) ;
#13213 = VECTOR ( 'NONE', #95, 1000.000000000000000 ) ;
#13214 = CARTESIAN_POINT ( 'NONE',  ( 2.789999999999999147, -8.936381166381891568E-14, 25.59481291497571220 ) ) ;
#13215 = CARTESIAN_POINT ( 'NONE',  ( 8.000000000000000000, -2.000000000000002665, 37.99999999999999289 ) ) ;
#13216 = ORIENTED_EDGE ( 'NONE', *, *, #13403, .F. ) ;
#13217 = CARTESIAN_POINT ( 'NONE',  ( 0.000000000000000000, -24.04302995059967429, 1.991882183130232242 ) ) ;
#13218 = FILL_AREA_STYLE_COLOUR ( '', #18960 ) ;
#13219 = CARTESIAN_POINT ( 'NONE',  ( 0.02436607992776108206, -24.15498966839966855, 5.391175441198523544 ) ) ;
#13220 = CARTESIAN_POINT ( 'NONE',  ( -15.19790265903627180, 9.644882309621941374, -32.00000000000000000 ) ) ;
#13221 = ORIENTED_EDGE ( 'NONE', *, *, #17895, .T. ) ;
#13222 = DIRECTION ( 'NONE',  ( -1.000000000000000000, -0.000000000000000000, -0.000000000000000000 ) ) ;
#13223 = ORIENTED_EDGE ( 'NONE', *, *, #15449, .T. ) ;
#13224 = PLANE ( 'NONE',  #15344 ) ;
#13225 = CARTESIAN_POINT ( 'NONE',  ( -3.350375938067097437, 4.611396867937201272, -10.31249999590322552 ) ) ;
#13226 = PRODUCT_DEFINITION_SHAPE ( 'NONE', 'NONE',  #12622 ) ;
#13227 = LINE ( 'NONE', #17924, #16682 ) ;
#13228 = LINE ( 'NONE', #13315, #10166 ) ;
#13229 = ORIENTED_EDGE ( 'NONE', *, *, #5059, .F. ) ;
#13230 = VECTOR ( 'NONE', #16883, 1000.000000000000000 ) ;
#13231 = CARTESIAN_POINT ( 'NONE',  ( -3.270778111535363131, -3.632567103900500971, -10.84374999795161543 ) ) ;
#13232 = CARTESIAN_POINT ( 'NONE',  ( 10.64522241986047568, 2.725425358843983450E-16, 5.700000000000002842 ) ) ;
#13233 = EDGE_LOOP ( 'NONE', ( #5099, #2438 ) ) ;
#13234 = AXIS2_PLACEMENT_3D ( 'NONE', #17057, #14146, #12357 ) ;
#13235 = EDGE_CURVE ( 'NONE', #12789, #4071, #14653, .T. ) ;
#13236 = DIRECTION ( 'NONE',  ( 0.000000000000000000, 0.000000000000000000, 1.000000000000000000 ) ) ;
#13237 = CARTESIAN_POINT ( 'NONE',  ( 0.1882238782932344479, 19.18368891937516452, -17.47009390565470000 ) ) ;
#13238 = EDGE_CURVE ( 'NONE', #4447, #16213, #6003, .T. ) ;
#13239 = ORIENTED_EDGE ( 'NONE', *, *, #16918, .F. ) ;
#13240 = CARTESIAN_POINT ( 'NONE',  ( 4.942249507334556924, 0.2590123213420971182, -13.34374999795161365 ) ) ;
#13241 = CARTESIAN_POINT ( 'NONE',  ( 2.620002426024508502, -5.142044285764769462, -9.500000000000005329 ) ) ;
#13242 = CARTESIAN_POINT ( 'NONE',  ( 8.468749997951615427, 2.873153789725825469, -3.954556930911862000 ) ) ;
#13243 = AXIS2_PLACEMENT_3D ( 'NONE', #13085, #11297, #13189 ) ;
#13244 = ORIENTED_EDGE ( 'NONE', *, *, #7127, .T. ) ;
#13245 = CARTESIAN_POINT ( 'NONE',  ( 2.789999999999999147, 5.391175441198615914, 24.15498966839965078 ) ) ;
#13246 = EDGE_LOOP ( 'NONE', ( #7899, #261 ) ) ;
#13247 = CARTESIAN_POINT ( 'NONE',  ( 0.000000000000000000, -1.991882183130475603, 24.04302995059966719 ) ) ;
#13248 = ORIENTED_EDGE ( 'NONE', *, *, #16075, .T. ) ;
#13249 = DIRECTION ( 'NONE',  ( 0.000000000000000000, 0.000000000000000000, -1.000000000000000000 ) ) ;
#13250 = FACE_OUTER_BOUND ( 'NONE', #7865, .T. ) ;
#13251 = VERTEX_POINT ( 'NONE', #4557 ) ;
#13252 = EDGE_CURVE ( 'NONE', #2117, #1278, #18558, .T. ) ;
#13253 = CARTESIAN_POINT ( 'NONE',  ( 3.499494075959791672, -3.499494075959840966, -8.968749997951611874 ) ) ;
#13254 = DIRECTION ( 'NONE',  ( 1.000000000000000000, 0.000000000000000000, 0.000000000000000000 ) ) ;
#13255 = CIRCLE ( 'NONE', #9413, 6.799999999999998934 ) ;
#13256 = FACE_OUTER_BOUND ( 'NONE', #13555, .T. ) ;
#13257 = EDGE_LOOP ( 'NONE', ( #2176, #17879, #1914, #15026 ) ) ;
#13258 = EDGE_CURVE ( 'NONE', #10948, #15013, #596, .T. ) ;
#13259 = CARTESIAN_POINT ( 'NONE',  ( 0.000000000000000000, 0.000000000000000000, -5.946610266546040968 ) ) ;
#13260 = ORIENTED_EDGE ( 'NONE', *, *, #6080, .T. ) ;
#13261 = CARTESIAN_POINT ( 'NONE',  ( 8.500000000000005329, 4.080749450109650844, -4.080749450109650844 ) ) ;
#13262 = CARTESIAN_POINT ( 'NONE',  ( -1.886022603841296830, 8.263794135966437014E-16, 6.735000000000022524 ) ) ;
#13263 = DIRECTION ( 'NONE',  ( -1.000000000000000000, -0.000000000000000000, -0.000000000000000000 ) ) ;
#13264 = EDGE_LOOP ( 'NONE', ( #15130, #10695, #12156, #16420 ) ) ;
#13265 = CARTESIAN_POINT ( 'NONE',  ( -3.846120219227901593, 3.114526743279308896, -11.96874999795161365 ) ) ;
#13266 =( NAMED_UNIT ( * ) SI_UNIT ( $, .STERADIAN. ) SOLID_ANGLE_UNIT ( ) );
#13267 = CARTESIAN_POINT ( 'NONE',  ( -1.185096637661215091, 5.575441324182695446, -7.000000000000005329 ) ) ;
#13268 = ORIENTED_EDGE ( 'NONE', *, *, #17983, .T. ) ;
#13269 = ORIENTED_EDGE ( 'NONE', *, *, #2834, .F. ) ;
#13270 = FACE_OUTER_BOUND ( 'NONE', #9326, .T. ) ;
#13271 = DIRECTION ( 'NONE',  ( 1.000000000000000000, -0.000000000000000000, -0.000000000000000000 ) ) ;
#13272 = VERTEX_POINT ( 'NONE', #6047 ) ;
#13273 = VECTOR ( 'NONE', #5173, 1000.000000000000000 ) ;
#13274 = DIRECTION ( 'NONE',  ( -0.000000000000000000, -0.000000000000000000, 1.000000000000000000 ) ) ;
#13275 = ORIENTED_EDGE ( 'NONE', *, *, #10615, .T. ) ;
#13276 = DIRECTION ( 'NONE',  ( -0.000000000000000000, -0.000000000000000000, 1.000000000000000000 ) ) ;
#13277 = CARTESIAN_POINT ( 'NONE',  ( 13.00000000000000000, -4.091807895435336739, 2.674798881044273546 ) ) ;
#13278 = VERTEX_POINT ( 'NONE', #12368 ) ;
#13279 = LINE ( 'NONE', #4274, #9123 ) ;
#13280 = DIRECTION ( 'NONE',  ( 1.000000000000000000, 0.000000000000000000, 0.000000000000000000 ) ) ;
#13281 = CARTESIAN_POINT ( 'NONE',  ( -7.937500000000000000, 4.582717761692651770, -0.7089489049740185234 ) ) ;
#13282 = FACE_OUTER_BOUND ( 'NONE', #8112, .T. ) ;
#13283 = LINE ( 'NONE', #16291, #12689 ) ;
#13284 = DIRECTION ( 'NONE',  ( 1.000000000000000000, 0.000000000000000000, 0.000000000000000000 ) ) ;
#13285 = CIRCLE ( 'NONE', #15207, 7.500000000000000000 ) ;
#13286 = ORIENTED_EDGE ( 'NONE', *, *, #15075, .T. ) ;
#13287 = DIRECTION ( 'NONE',  ( -0.000000000000000000, -0.000000000000000000, 1.000000000000000000 ) ) ;
#13288 = CYLINDRICAL_SURFACE ( 'NONE', #5534, 28.06981291497571362 ) ;
#13289 = DIRECTION ( 'NONE',  ( 1.000000000000000000, 0.000000000000000000, 0.000000000000000000 ) ) ;
#13290 = DIRECTION ( 'NONE',  ( -1.000000000000000000, 0.000000000000000000, -0.000000000000000000 ) ) ;
#13291 = CARTESIAN_POINT ( 'NONE',  ( -3.954556930911862000, 2.873153789725825469, -8.843749997951615427 ) ) ;
#13292 = EDGE_CURVE ( 'NONE', #12779, #16239, #18481, .T. ) ;
#13293 = VERTEX_POINT ( 'NONE', #15166 ) ;
#13294 = CYLINDRICAL_SURFACE ( 'NONE', #16680, 1.000000000000002665 ) ;
#13295 = DIRECTION ( 'NONE',  ( 1.000000000000000000, 0.000000000000000000, 0.000000000000000000 ) ) ;
#13296 = ORIENTED_EDGE ( 'NONE', *, *, #17579, .F. ) ;
#13297 = CARTESIAN_POINT ( 'NONE',  ( 9.343749997951615427, 1.280903732194421218, 4.780397808154266848 ) ) ;
#13298 = AXIS2_PLACEMENT_3D ( 'NONE', #6101, #12223, #18036 ) ;
#13299 = CARTESIAN_POINT ( 'NONE',  ( 0.000000000000000000, 12.52067188844379864, -20.62201879784900882 ) ) ;
#13300 = CARTESIAN_POINT ( 'NONE',  ( -16.96448111170888851, 1.130229351527647808, -32.00000000000000000 ) ) ;
#13301 = CARTESIAN_POINT ( 'NONE',  ( -10.00000000000000000, 0.000000000000000000, 0.000000000000000000 ) ) ;
#13302 = ORIENTED_EDGE ( 'NONE', *, *, #1295, .F. ) ;
#13303 = DIRECTION ( 'NONE',  ( 0.7071067811865489050, 0.000000000000000000, -0.7071067811865462405 ) ) ;
#13304 = CARTESIAN_POINT ( 'NONE',  ( 4.465502636338039011, 1.988169868018562436, -8.843749997951615427 ) ) ;
#13305 = EDGE_CURVE ( 'NONE', #9061, #12845, #4855, .T. ) ;
#13306 = CARTESIAN_POINT ( 'NONE',  ( 10.50000000000000711, -5.700000000000005507, 0.9027913098498173694 ) ) ;
#13307 = ORIENTED_EDGE ( 'NONE', *, *, #15225, .F. ) ;
#13308 = DIRECTION ( 'NONE',  ( -1.000000000000000000, -0.000000000000000000, -0.000000000000000000 ) ) ;
#13309 = VECTOR ( 'NONE', #18793, 1000.000000000000000 ) ;
#13310 = ORIENTED_EDGE ( 'NONE', *, *, #12607, .F. ) ;
#13311 = CARTESIAN_POINT ( 'NONE',  ( -10.58013454126452224, -14.56230589874905235, -32.00000000000000000 ) ) ;
#13312 = AXIS2_PLACEMENT_3D ( 'NONE', #17900, #16404, #8798 ) ;
#13313 = CARTESIAN_POINT ( 'NONE',  ( 5.000000000000000000, 0.000000000000000000, 41.99999999999999289 ) ) ;
#13314 = FACE_OUTER_BOUND ( 'NONE', #13626, .T. ) ;
#13315 = CARTESIAN_POINT ( 'NONE',  ( 8.000000000000000000, -2.000000000000002665, 37.99999999999999289 ) ) ;
#13316 = EDGE_CURVE ( 'NONE', #14880, #619, #4594, .T. ) ;
#13317 = ORIENTED_EDGE ( 'NONE', *, *, #3087, .F. ) ;
#13318 = CYLINDRICAL_SURFACE ( 'NONE', #2592, 1.000000000000002665 ) ;
#13319 = DIRECTION ( 'NONE',  ( 0.000000000000000000, 0.000000000000000000, -1.000000000000000000 ) ) ;
#13320 = ORIENTED_EDGE ( 'NONE', *, *, #19346, .T. ) ;
#13321 = B_SPLINE_CURVE_WITH_KNOTS ( 'NONE', 3,
 ( #19590, #8892, #3995, #11597, #17698, #5482, #14896, #4288 ),
 .UNSPECIFIED., .F., .F.,
 ( 4, 2, 2, 4 ),
 ( 0.004637198101876866679, 0.005792104118025186155, 0.006947010134173505630, 0.009256822166470144581 ),
 .UNSPECIFIED. ) ;
#13322 = AXIS2_PLACEMENT_3D ( 'NONE', #15137, #9237, #7308 ) ;
#13323 = AXIS2_PLACEMENT_3D ( 'NONE', #12215, #2898, #8815 ) ;
#13324 = CARTESIAN_POINT ( 'NONE',  ( 1.303212546021007334, 8.413025409128788823, -0.3142460757452215092 ) ) ;
#13325 = DIRECTION ( 'NONE',  ( 0.000000000000000000, 0.000000000000000000, 1.000000000000000000 ) ) ;
#13326 = ORIENTED_EDGE ( 'NONE', *, *, #2961, .F. ) ;
#13327 = CARTESIAN_POINT ( 'NONE',  ( 1.988169868018593300, 4.465502636338023912, -9.468749997951615427 ) ) ;
#13328 = CARTESIAN_POINT ( 'NONE',  ( 11.81249999590322552, 3.631840208645794821, 4.484949146646379781 ) ) ;
#13329 = DIRECTION ( 'NONE',  ( 0.000000000000000000, 0.000000000000000000, 1.000000000000000000 ) ) ;
#13330 = VERTEX_POINT ( 'NONE', #349 ) ;
#13331 = ADVANCED_FACE ( 'NONE', ( #6433 ), #4443, .T. ) ;
#13332 = CARTESIAN_POINT ( 'NONE',  ( 2.999999999999998224, 3.950217066951266176, 3.681818181818181213 ) ) ;
#13333 = ORIENTED_EDGE ( 'NONE', *, *, #6204, .F. ) ;
#13334 = CARTESIAN_POINT ( 'NONE',  ( -2.255998204157477538, -17.85806462366060288, 32.00000000000000000 ) ) ;
#13335 = ORIENTED_EDGE ( 'NONE', *, *, #14969, .F. ) ;
#13336 = DIRECTION ( 'NONE',  ( 1.000000000000000000, 0.000000000000000000, 0.000000000000000000 ) ) ;
#13337 = DIRECTION ( 'NONE',  ( 1.000000000000000000, 0.000000000000000000, 0.000000000000000000 ) ) ;
#13338 = CARTESIAN_POINT ( 'NONE',  ( 4.888101187499994893, -0.7741991708319229115, -6.968749997951614539 ) ) ;
#13339 = CARTESIAN_POINT ( 'NONE',  ( 8.968749997951611874, -4.780397808154247308, -1.280903732194487166 ) ) ;
#13340 = EDGE_CURVE ( 'NONE', #5005, #1162, #15345, .T. ) ;
#13341 = AXIS2_PLACEMENT_3D ( 'NONE', #17329, #128, #12634 ) ;
#13342 = DIRECTION ( 'NONE',  ( 1.000000000000000000, 0.000000000000000000, 0.000000000000000000 ) ) ;
#13343 = CIRCLE ( 'NONE', #19083, 1.000000000000000888 ) ;
#13344 = ORIENTED_EDGE ( 'NONE', *, *, #11308, .F. ) ;
#13345 = ADVANCED_FACE ( 'NONE', ( #15563 ), #11059, .F. ) ;
#13346 = CARTESIAN_POINT ( 'NONE',  ( 13.86923836996420789, -11.47363181547641453, 32.00000000000000000 ) ) ;
#13347 = ORIENTED_EDGE ( 'NONE', *, *, #7855, .F. ) ;
#13348 = DIRECTION ( 'NONE',  ( 0.000000000000000000, -1.000000000000000000, 0.000000000000000000 ) ) ;
#13349 = ADVANCED_FACE ( 'NONE', ( #1559 ), #5701, .T. ) ;
#13350 = CARTESIAN_POINT ( 'NONE',  ( 8.000000000000000000, 0.000000000000000000, 0.000000000000000000 ) ) ;
#13351 = CARTESIAN_POINT ( 'NONE',  ( 4.235925505221166176, 3.814044456245473835, -7.000000000000005329 ) ) ;
#13352 = AXIS2_PLACEMENT_3D ( 'NONE', #18536, #18833, #17336 ) ;
#13353 = FACE_OUTER_BOUND ( 'NONE', #18606, .T. ) ;
#13354 = ORIENTED_EDGE ( 'NONE', *, *, #17655, .T. ) ;
#13355 = CYLINDRICAL_SURFACE ( 'NONE', #18984, 1.000000000000000888 ) ;
#13356 = EDGE_CURVE ( 'NONE', #1041, #7654, #18188, .T. ) ;
#13357 = CARTESIAN_POINT ( 'NONE',  ( -0.5109457054262123155, -4.861323657744403448, -8.468749997951615427 ) ) ;
#13358 = CYLINDRICAL_SURFACE ( 'NONE', #9280, 1.000000000000004441 ) ;
#13359 = EDGE_CURVE ( 'NONE', #6326, #4605, #4756, .T. ) ;
#13360 = ORIENTED_EDGE ( 'NONE', *, *, #7312, .F. ) ;
#13361 = ORIENTED_EDGE ( 'NONE', *, *, #3354, .T. ) ;
#13362 = DIRECTION ( 'NONE',  ( 1.000000000000000000, 0.000000000000000000, 0.000000000000000000 ) ) ;
#13363 = CARTESIAN_POINT ( 'NONE',  ( 10.46874999795161720, -1.016293382781444654, 4.781284448697187273 ) ) ;
#13364 = ORIENTED_EDGE ( 'NONE', *, *, #16965, .F. ) ;
#13365 = EDGE_CURVE ( 'NONE', #13931, #4794, #9966, .T. ) ;
#13366 = FACE_OUTER_BOUND ( 'NONE', #16312, .T. ) ;
#13367 = ORIENTED_EDGE ( 'NONE', *, *, #5279, .F. ) ;
#13368 = CARTESIAN_POINT ( 'NONE',  ( -3.255998204157480203, -17.85806462366060288, 32.00000000000000000 ) ) ;
#13369 = CARTESIAN_POINT ( 'NONE',  ( 2.789999999999999147, -20.70663861606260170, -15.04425356660783031 ) ) ;
#13370 = ORIENTED_EDGE ( 'NONE', *, *, #14224, .F. ) ;
#13371 = CARTESIAN_POINT ( 'NONE',  ( 2.789999999999999147, 23.48180575137730131, 5.535312321042802353 ) ) ;
#13372 = EDGE_CURVE ( 'NONE', #15740, #6118, #16761, .T. ) ;
#13373 = FACE_OUTER_BOUND ( 'NONE', #7169, .T. ) ;
#13374 = DIRECTION ( 'NONE',  ( 1.000000000000000000, 0.000000000000000000, 0.000000000000000000 ) ) ;
#13375 = DIRECTION ( 'NONE',  ( 0.000000000000000000, 0.000000000000000000, 1.000000000000000000 ) ) ;
#13376 = PRODUCT_DEFINITION_SHAPE ( 'NONE', 'NONE',  #19785 ) ;
#13377 = EDGE_CURVE ( 'NONE', #4037, #12535, #8582, .T. ) ;
#13378 = VECTOR ( 'NONE', #12614, 1000.000000000000000 ) ;
#13379 = DIRECTION ( 'NONE',  ( -1.000000000000000000, -0.000000000000000000, -0.000000000000000000 ) ) ;
#13380 =( NAMED_UNIT ( * ) SI_UNIT ( $, .STERADIAN. ) SOLID_ANGLE_UNIT ( ) );
#13381 = DIRECTION ( 'NONE',  ( -1.000000000000000000, -0.000000000000000000, -0.000000000000000000 ) ) ;
#13382 = VERTEX_POINT ( 'NONE', #8154 ) ;
#13383 = CARTESIAN_POINT ( 'NONE',  ( -15.28688694438835505, -7.664027248171298545, 32.00000000000000000 ) ) ;
#13384 = CARTESIAN_POINT ( 'NONE',  ( -17.96448111170888851, 1.130229351527647585, -32.00000000000000000 ) ) ;
#13385 = UNCERTAINTY_MEASURE_WITH_UNIT (LENGTH_MEASURE( 1.000000000000000082E-05 ), #3786, 'distance_accuracy_value', 'NONE');
#13386 = DIRECTION ( 'NONE',  ( 0.000000000000000000, 0.000000000000000000, 1.000000000000000000 ) ) ;
#13387 = B_SPLINE_CURVE_WITH_KNOTS ( 'NONE', 3,
 ( #12212, #16720, #2999, #14405, #3692, #17110 ),
 .UNSPECIFIED., .F., .F.,
 ( 4, 2, 4 ),
 ( 2.586195665699493951E-07, 0.001878649493629688805, 0.003757040367692807744 ),
 .UNSPECIFIED. ) ;
#13388 = FACE_OUTER_BOUND ( 'NONE', #3768, .T. ) ;
#13389 = FACE_OUTER_BOUND ( 'NONE', #9255, .T. ) ;
#13390 = EDGE_LOOP ( 'NONE', ( #13034, #8293 ) ) ;
#13391 = CARTESIAN_POINT ( 'NONE',  ( 1.039999999999996705, -27.68468304288255410, -4.633866840649218055 ) ) ;
#13392 = DIRECTION ( 'NONE',  ( -1.000000000000000000, -0.000000000000000000, -0.000000000000000000 ) ) ;
#13393 = ORIENTED_EDGE ( 'NONE', *, *, #11170, .T. ) ;
#13394 = CARTESIAN_POINT ( 'NONE',  ( 13.31249999590322730, -4.235925505221167064, 3.814044456245474279 ) ) ;
#13395 = EDGE_CURVE ( 'NONE', #18268, #17360, #17959, .T. ) ;
#13396 = CARTESIAN_POINT ( 'NONE',  ( 12.81249999590322552, -2.068159791354146293, -5.387740456496247887 ) ) ;
#13397 = DIRECTION ( 'NONE',  ( 1.000000000000000000, -0.000000000000000000, -0.000000000000000000 ) ) ;
#13398 = DIRECTION ( 'NONE',  ( 0.000000000000000000, -1.000000000000000000, 0.000000000000000000 ) ) ;
#13399 = ORIENTED_EDGE ( 'NONE', *, *, #8457, .F. ) ;
#13400 = DIRECTION ( 'NONE',  ( 0.000000000000000000, 0.000000000000000000, -1.000000000000000000 ) ) ;
#13401 = FILL_AREA_STYLE ('',( #13218 ) ) ;
#13402 = DIRECTION ( 'NONE',  ( 1.000000000000000000, 0.000000000000000000, 0.000000000000000000 ) ) ;
#13403 = EDGE_CURVE ( 'NONE', #196, #14221, #15949, .T. ) ;
#13404 = VERTEX_POINT ( 'NONE', #15962 ) ;
#13405 = CARTESIAN_POINT ( 'NONE',  ( 2.789999999999999147, 24.04302995059966364, -1.991882183130384121 ) ) ;
#13406 = ORIENTED_EDGE ( 'NONE', *, *, #9117, .F. ) ;
#13407 = CARTESIAN_POINT ( 'NONE',  ( 2.789999999999999147, -20.62201879784904079, -12.52067188844374179 ) ) ;
#13408 = CARTESIAN_POINT ( 'NONE',  ( 8.468749997951615427, 2.873153789725825469, -3.954556930911862000 ) ) ;
#13409 = CARTESIAN_POINT ( 'NONE',  ( -90.00000000000000000, 0.000000000000000000, 0.000000000000000000 ) ) ;
#13410 = AXIS2_PLACEMENT_3D ( 'NONE', #12341, #12537, #16945 ) ;
#13411 = EDGE_CURVE ( 'NONE', #4459, #17830, #14984, .T. ) ;
#13412 = CARTESIAN_POINT ( 'NONE',  ( 5.700000000000001066, 0.000000000000000000, -13.97977757194595760 ) ) ;
#13413 = AXIS2_PLACEMENT_3D ( 'NONE', #4626, #6502, #7819 ) ;
#13414 = ORIENTED_EDGE ( 'NONE', *, *, #3586, .F. ) ;
#13415 = CARTESIAN_POINT ( 'NONE',  ( -2.500000000000002220, 0.000000000000000000, -6.543750000000023270 ) ) ;
#13416 = EDGE_LOOP ( 'NONE', ( #17605, #16558, #9364, #17479 ) ) ;
#13417 = CARTESIAN_POINT ( 'NONE',  ( -0.000000000000000000, -8.000000000000003553, 41.99999999999999289 ) ) ;
#13418 = CARTESIAN_POINT ( 'NONE',  ( -3.383411828340740850E-14, -4.888101187500000222, -11.84374999795161365 ) ) ;
#13419 = ORIENTED_EDGE ( 'NONE', *, *, #4199, .F. ) ;
#13421 = CARTESIAN_POINT ( 'NONE',  ( 5.207209108562838473, 2.318398865532038666, -8.000000000000005329 ) ) ;
#13420 = AXIS2_PLACEMENT_3D ( 'NONE', #7262, #12093, #16595 ) ;
#13422 = B_SPLINE_CURVE_WITH_KNOTS ( 'NONE', 3,
 ( #11025, #3513, #9630, #15627, #15723, #3321 ),
 .UNSPECIFIED., .F., .F.,
 ( 4, 2, 4 ),
 ( 4.462636732861209103E-07, 0.001879885066975070214, 0.003759323870276854232 ),
 .UNSPECIFIED. ) ;
#13423 = CARTESIAN_POINT ( 'NONE',  ( 11.34374999795161543, 3.114526743279256493, 3.846120219227944670 ) ) ;
#13424 = AXIS2_PLACEMENT_3D ( 'NONE', #12503, #15510, #17203 ) ;
#13425 = FACE_BOUND ( 'NONE', #15314, .T. ) ;
#13426 = ADVANCED_FACE ( 'NONE', ( #6634 ), #2249, .T. ) ;
#13427 = EDGE_LOOP ( 'NONE', ( #12441, #10567 ) ) ;
#13428 = CARTESIAN_POINT ( 'NONE',  ( 0.6764999999999817826, 0.000000000000000000, 4.000000000000000000 ) ) ;
#13429 = VERTEX_POINT ( 'NONE', #9667 ) ;
#13430 = CARTESIAN_POINT ( 'NONE',  ( 2.030753610301991419, 19.86438386685660618, 19.12676442129351173 ) ) ;
#13431 = VERTEX_POINT ( 'NONE', #11461 ) ;
#13432 = DIRECTION ( 'NONE',  ( 0.000000000000000000, 0.000000000000000000, 1.000000000000000000 ) ) ;
#13433 = CARTESIAN_POINT ( 'NONE',  ( 2.765633920072242624, 9.836394144775706394, 22.71065055754456097 ) ) ;
#13434 = DIRECTION ( 'NONE',  ( 0.000000000000000000, 0.000000000000000000, 1.000000000000000000 ) ) ;
#13435 = CARTESIAN_POINT ( 'NONE',  ( 10.50000000000000711, -3.631840208645764179, -4.484949146646406426 ) ) ;
#13436 = CARTESIAN_POINT ( 'NONE',  ( 6.626241948324199882, -16.73597674598852691, 32.00000000000000000 ) ) ;
#13437 = ORIENTED_EDGE ( 'NONE', *, *, #17088, .F. ) ;
#13438 = DIRECTION ( 'NONE',  ( 0.000000000000000000, 0.000000000000000000, -1.000000000000000000 ) ) ;
#13439 = AXIS2_PLACEMENT_3D ( 'NONE', #16906, #3580, #9704 ) ;
#13440 = FACE_BOUND ( 'NONE', #16169, .T. ) ;
#13441 = EDGE_CURVE ( 'NONE', #18420, #15528, #1562, .T. ) ;
#13442 = EDGE_CURVE ( 'NONE', #8517, #5549, #6342, .T. ) ;
#13443 = ORIENTED_EDGE ( 'NONE', *, *, #19346, .F. ) ;
#13444 = DIRECTION ( 'NONE',  ( -6.419766481290786633E-33, 1.000000000000000000, 0.000000000000000000 ) ) ;
#13445 = FACE_BOUND ( 'NONE', #5017, .T. ) ;
#13446 = CARTESIAN_POINT ( 'NONE',  ( 5.575441324182689229, -1.185096637661254171, -10.00000000000000533 ) ) ;
#13447 = CARTESIAN_POINT ( 'NONE',  ( 2.718131853594931258, -21.92302674874953539, -12.74240566899008442 ) ) ;
#13448 = EDGE_LOOP ( 'NONE', ( #6491, #19058, #19049, #2694 ) ) ;
#13449 = CARTESIAN_POINT ( 'NONE',  ( 1.280903732194454303, 4.780397808154257078, -8.968749997951613651 ) ) ;
#13450 = AXIS2_PLACEMENT_3D ( 'NONE', #14858, #9801, #2178 ) ;
#13451 = DIRECTION ( 'NONE',  ( -1.000000000000000000, 6.982962677686266711E-15, 0.000000000000000000 ) ) ;
#13452 = CARTESIAN_POINT ( 'NONE',  ( -2.695436003842760275, -4.150607464521772094, -9.968749997951617203 ) ) ;
#13453 = DIRECTION ( 'NONE',  ( 0.000000000000000000, 0.000000000000000000, -1.000000000000000000 ) ) ;
#13454 = VECTOR ( 'NONE', #18051, 1000.000000000000000 ) ;
#13455 = ORIENTED_EDGE ( 'NONE', *, *, #11626, .T. ) ;
#13456 = ORIENTED_EDGE ( 'NONE', *, *, #7489, .F. ) ;
#13457 = DIRECTION ( 'NONE',  ( 1.000000000000000000, -0.000000000000000000, -0.000000000000000000 ) ) ;
#13458 = CARTESIAN_POINT ( 'NONE',  ( 10.50000000000000711, -2.068159791354221344, 5.387740456496221242 ) ) ;
#13459 = ORIENTED_EDGE ( 'NONE', *, *, #4079, .F. ) ;
#13460 = DIRECTION ( 'NONE',  ( 0.000000000000000000, 0.000000000000000000, -1.000000000000000000 ) ) ;
#13461 = ORIENTED_EDGE ( 'NONE', *, *, #607, .F. ) ;
#13462 = DIRECTION ( 'NONE',  ( -0.000000000000000000, -0.000000000000000000, 1.000000000000000000 ) ) ;
#13463 = SHAPE_REPRESENTATION ( 'Outer Wheel Hub Shell', ( #16724 ), #7108 ) ;
#13464 = FACE_OUTER_BOUND ( 'NONE', #2383, .T. ) ;
#13465 = PRODUCT_RELATED_PRODUCT_CATEGORY ( 'part', '', ( #2506 ) ) ;
#13466 = AXIS2_PLACEMENT_3D ( 'NONE', #5612, #11728, #15128 ) ;
#13467 = ORIENTED_EDGE ( 'NONE', *, *, #13201, .T. ) ;
#13468 = CIRCLE ( 'NONE', #15079, 6.000000000000000000 ) ;
#13469 = AXIS2_PLACEMENT_3D ( 'NONE', #2124, #13032, #11620 ) ;
#13470 = EDGE_CURVE ( 'NONE', #16599, #4088, #6492, .T. ) ;
#13471 = DIRECTION ( 'NONE',  ( -1.000000000000000000, -0.000000000000000000, -0.000000000000000000 ) ) ;
#13472 = CARTESIAN_POINT ( 'NONE',  ( 7.312499995903225525, 0.000000000000000000, -5.700000000000001066 ) ) ;
#13473 = FACE_OUTER_BOUND ( 'NONE', #6995, .T. ) ;
#13474 = ADVANCED_FACE ( 'NONE', ( #6932 ), #12315, .T. ) ;
#13475 = ORIENTED_EDGE ( 'NONE', *, *, #3139, .F. ) ;
#13476 = DIRECTION ( 'NONE',  ( 0.000000000000000000, 0.000000000000000000, 1.000000000000000000 ) ) ;
#13477 = PRESENTATION_STYLE_ASSIGNMENT (( #1478 ) ) ;
#13478 = DIRECTION ( 'NONE',  ( -0.000000000000000000, -0.000000000000000000, 1.000000000000000000 ) ) ;
#13479 = ORIENTED_EDGE ( 'NONE', *, *, #11062, .T. ) ;
#13480 = CARTESIAN_POINT ( 'NONE',  ( 7.078124996927420476, -3.696815770993907903E-14, 5.294050593750000644 ) ) ;
#13481 = CARTESIAN_POINT ( 'NONE',  ( -3.476417968967383754, 17.43449690031536292, 35.00000000000000000 ) ) ;
#13482 = AXIS2_PLACEMENT_3D ( 'NONE', #15474, #9174, #5956 ) ;
#13483 = CARTESIAN_POINT ( 'NONE',  ( 7.937500000000000000, 4.582717761692648217, -6.527800000000000047 ) ) ;
#13484 = EDGE_CURVE ( 'NONE', #12580, #2419, #2532, .T. ) ;
#13485 = AXIS2_PLACEMENT_3D ( 'NONE', #17384, #5069, #780 ) ;
#13486 = DIRECTION ( 'NONE',  ( -1.000000000000000000, 0.000000000000000000, 0.000000000000000000 ) ) ;
#13487 = CARTESIAN_POINT ( 'NONE',  ( -5.574407415329178939, -1.493657965219446382, -9.812499995903223748 ) ) ;
#13488 = ORIENTED_EDGE ( 'NONE', *, *, #8486, .F. ) ;
#13489 = CARTESIAN_POINT ( 'NONE',  ( 0.02436607992775544421, -22.71065055754445439, -9.836394144775947979 ) ) ;
#13490 = CIRCLE ( 'NONE', #65, 1.000000000000004441 ) ;
#13491 = DIRECTION ( 'NONE',  ( -0.000000000000000000, -0.000000000000000000, 1.000000000000000000 ) ) ;
#13492 = EDGE_LOOP ( 'NONE', ( #13399, #18173, #15101, #17646 ) ) ;
#13493 = DIRECTION ( 'NONE',  ( 0.000000000000000000, 0.000000000000000000, -1.000000000000000000 ) ) ;
#13494 = EDGE_CURVE ( 'NONE', #540, #18318, #19761, .T. ) ;
#13495 = CARTESIAN_POINT ( 'NONE',  ( 15.31249999590322552, 2.318398865532109276, -5.207209108562804722 ) ) ;
#13496 = AXIS2_PLACEMENT_3D ( 'NONE', #5177, #11296, #15991 ) ;
#13497 = AXIS2_PLACEMENT_3D ( 'NONE', #14471, #9570, #17172 ) ;
#13498 = AXIS2_PLACEMENT_3D ( 'NONE', #2030, #3135, #11039 ) ;
#13499 = CARTESIAN_POINT ( 'NONE',  ( 2.262072661820534236, -26.82026385750180353, 3.461047254864169975 ) ) ;
#13500 = DIRECTION ( 'NONE',  ( 0.000000000000000000, 0.000000000000000000, 1.000000000000000000 ) ) ;
#13501 = ORIENTED_EDGE ( 'NONE', *, *, #6423, .T. ) ;
#13502 = AXIS2_PLACEMENT_3D ( 'NONE', #10752, #9351, #10458 ) ;
#13503 = DIRECTION ( 'NONE',  ( -6.419766481290786633E-33, 1.000000000000000000, 0.000000000000000000 ) ) ;
#13504 = CARTESIAN_POINT ( 'NONE',  ( 2.999999999999998224, -3.218695387886217674, 2.999999999999999112 ) ) ;
#13505 = CIRCLE ( 'NONE', #5503, 4.400000000000000355 ) ;
#13506 = DIRECTION ( 'NONE',  ( 0.000000000000000000, 0.000000000000000000, 1.000000000000000000 ) ) ;
#13507 = VERTEX_POINT ( 'NONE', #10446 ) ;
#13508 = CARTESIAN_POINT ( 'NONE',  ( -20.63749999999999574, 0.000000000000000000, -6.799999999999998046 ) ) ;
#13509 = EDGE_LOOP ( 'NONE', ( #15334, #17926, #13758, #5106 ) ) ;
#13510 = CARTESIAN_POINT ( 'NONE',  ( -18.96448111170889206, 1.130229351527647808, 35.00000000000000000 ) ) ;
#13511 = CARTESIAN_POINT ( 'NONE',  ( 11.84374999795161365, 4.888101187500000222, -2.993098736590125853E-16 ) ) ;
#13512 = EDGE_CURVE ( 'NONE', #11113, #298, #16549, .T. ) ;
#13513 = CARTESIAN_POINT ( 'NONE',  ( 2.718131847775118182, 24.78765742476139522, 5.344160105508784397 ) ) ;
#13514 = MECHANICAL_DESIGN_GEOMETRIC_PRESENTATION_REPRESENTATION (  '', ( #8729 ), #11295 ) ;
#13515 = DIRECTION ( 'NONE',  ( 1.000000000000000000, 0.000000000000000000, 0.000000000000000000 ) ) ;
#13516 = ORIENTED_EDGE ( 'NONE', *, *, #9552, .F. ) ;
#13517 = CARTESIAN_POINT ( 'NONE',  ( -4.233219804643904460, -2.444050593749961031, -11.84374999795161365 ) ) ;
#13518 = CARTESIAN_POINT ( 'NONE',  ( 0.07186813532171011654, 25.22589920183360945, 2.577209017047096484 ) ) ;
#13519 = EDGE_CURVE ( 'NONE', #8838, #8958, #5725, .T. ) ;
#13520 = ORIENTED_EDGE ( 'NONE', *, *, #1740, .T. ) ;
#13521 = CIRCLE ( 'NONE', #2977, 24.12539914357697413 ) ;
#13522 = CIRCLE ( 'NONE', #10971, 4.500000000000000000 ) ;
#13523 = CARTESIAN_POINT ( 'NONE',  ( 2.246813503491833508, 4.409619785863906571, -12.96874999795161543 ) ) ;
#13524 = DIRECTION ( 'NONE',  ( 9.559896011775280412E-17, -0.7806247497997995666, -0.6250000000000001110 ) ) ;
#13525 = ORIENTED_EDGE ( 'NONE', *, *, #7351, .T. ) ;
#13526 = APPLICATION_CONTEXT ( 'automotive_design' ) ;
#13527 = CARTESIAN_POINT ( 'NONE',  ( 4.780397808154257078, -1.280903732194453859, -13.96874999795161365 ) ) ;
#13528 = CARTESIAN_POINT ( 'NONE',  ( 14.84374999795161543, -1.988169868018592412, 4.465502636338025688 ) ) ;
#13529 = CYLINDRICAL_SURFACE ( 'NONE', #14523, 10.00000000000000000 ) ;
#13530 = ORIENTED_EDGE ( 'NONE', *, *, #4850, .T. ) ;
#13531 = CYLINDRICAL_SURFACE ( 'NONE', #7980, 2.524999999999995914 ) ;
#13532 = EDGE_LOOP ( 'NONE', ( #9965, #18162 ) ) ;
#13533 = CARTESIAN_POINT ( 'NONE',  ( -15.00000000000000355, -3.434748899119118626, 2.750000000000001332 ) ) ;
#13534 = VERTEX_POINT ( 'NONE', #11840 ) ;
#13535 = CARTESIAN_POINT ( 'NONE',  ( 1.039999999999995373, 25.12109765559670649, -12.52377138324197681 ) ) ;
#13536 = AXIS2_PLACEMENT_3D ( 'NONE', #11904, #2888, #9003 ) ;
#13537 = DIRECTION ( 'NONE',  ( -1.000000000000000000, 0.000000000000000000, 0.000000000000000000 ) ) ;
#13538 = EDGE_CURVE ( 'NONE', #344, #12048, #12104, .T. ) ;
#13539 = CARTESIAN_POINT ( 'NONE',  ( 4.409619785863891472, -2.246813503491864150, -7.968749997951616315 ) ) ;
#13540 = CARTESIAN_POINT ( 'NONE',  ( 12.00000000000000533, -1.185096637661177343, -5.575441324182703440 ) ) ;
#13541 = CARTESIAN_POINT ( 'NONE',  ( -2.000000000000001776, 0.000000000000000000, 4.000000000000000000 ) ) ;
#13542 = ORIENTED_EDGE ( 'NONE', *, *, #631, .T. ) ;
#13543 = FACE_OUTER_BOUND ( 'NONE', #14260, .T. ) ;
#13544 = CIRCLE ( 'NONE', #6541, 6.000000000000020428 ) ;
#13545 = EDGE_CURVE ( 'NONE', #9982, #6802, #7414, .T. ) ;
#13546 = PLANE ( 'NONE',  #5892 ) ;
#13547 = VERTEX_POINT ( 'NONE', #2727 ) ;
#13548 = AXIS2_PLACEMENT_3D ( 'NONE', #18496, #17005, #9405 ) ;
#13549 = DIRECTION ( 'NONE',  ( -0.000000000000000000, -0.000000000000000000, -1.000000000000000000 ) ) ;
#13550 = FACE_OUTER_BOUND ( 'NONE', #15635, .T. ) ;
#13551 = ORIENTED_EDGE ( 'NONE', *, *, #4165, .F. ) ;
#13552 = DIRECTION ( 'NONE',  ( 0.000000000000000000, 1.224646799147333486E-16, 1.000000000000000000 ) ) ;
#13553 = CARTESIAN_POINT ( 'NONE',  ( 2.695436003842704764, -4.150607464521812062, -12.96874999795161543 ) ) ;
#13554 = DIRECTION ( 'NONE',  ( -0.8660254037844418162, 0.4999999999999944489, 0.000000000000000000 ) ) ;
#13555 = EDGE_LOOP ( 'NONE', ( #13892, #16033, #4940, #18584 ) ) ;
#13556 = DIRECTION ( 'NONE',  ( -0.000000000000000000, -0.000000000000000000, 1.000000000000000000 ) ) ;
#13557 = AXIS2_PLACEMENT_3D ( 'NONE', #3840, #19143, #10058 ) ;
#13558 = ORIENTED_EDGE ( 'NONE', *, *, #16355, .T. ) ;
#13559 = CARTESIAN_POINT ( 'NONE',  ( 0.000000000000000000, 0.000000000000000000, -48.31780000000000541 ) ) ;
#13560 = CARTESIAN_POINT ( 'NONE',  ( 5.763142191869157216, 0.3020334839682475847, -12.50000000000000533 ) ) ;
#13561 = CARTESIAN_POINT ( 'NONE',  ( -4.476417968967385974, 17.43449690031536292, -35.00000000000000000 ) ) ;
#13562 = ORIENTED_EDGE ( 'NONE', *, *, #3156, .F. ) ;
#13563 = EDGE_CURVE ( 'NONE', #6039, #9260, #8273, .T. ) ;
#13564 = ORIENTED_EDGE ( 'NONE', *, *, #18821, .T. ) ;
#13565 = CARTESIAN_POINT ( 'NONE',  ( 2.444050593750020095, 4.233219804643871598, -6.656249997951614539 ) ) ;
#13566 = CARTESIAN_POINT ( 'NONE',  ( 0.5109457054261780096, 4.861323657744407001, -8.843749997951615427 ) ) ;
#13568 = ORIENTED_EDGE ( 'NONE', *, *, #18988, .T. ) ;
#13567 = TOROIDAL_SURFACE ( 'NONE', #6841, 24.12539914357697413, 8.000000000000000000 ) ;
#13569 = DIRECTION ( 'NONE',  ( 1.000000000000000000, 0.000000000000000000, 0.000000000000000000 ) ) ;
#13570 = ORIENTED_EDGE ( 'NONE', *, *, #11587, .T. ) ;
#13571 = EDGE_CURVE ( 'NONE', #2365, #9172, #7949, .T. ) ;
#13572 = DIRECTION ( 'NONE',  ( 1.000000000000000000, 0.000000000000000000, 0.000000000000000000 ) ) ;
#13573 = DIRECTION ( 'NONE',  ( -1.000000000000000000, 0.000000000000000000, 0.000000000000000000 ) ) ;
#13574 = PRESENTATION_LAYER_ASSIGNMENT (  '', '', ( #11019 ) ) ;
#13575 = EDGE_LOOP ( 'NONE', ( #10865, #18681, #835, #13770, #15071 ) ) ;
#13576 = CARTESIAN_POINT ( 'NONE',  ( 2.789999999999999147, 9.324097380959765147, -22.25075486061728824 ) ) ;
#13577 = CARTESIAN_POINT ( 'NONE',  ( 8.312499995903225525, 1.761396867937200517, -5.421022142882375938 ) ) ;
#13578 = CARTESIAN_POINT ( 'NONE',  ( -3.945386292505473391E-14, -5.700000000000001066, -12.31249999590322552 ) ) ;
#13579 = ORIENTED_EDGE ( 'NONE', *, *, #1520, .F. ) ;
#13580 = CARTESIAN_POINT ( 'NONE',  ( 2.789999999999999147, -9.324097380959294412, -22.25075486061747654 ) ) ;
#13581 = CARTESIAN_POINT ( 'NONE',  ( 12.32184790671639618, 13.12143529358541016, -32.00000000000000000 ) ) ;
#13582 = VERTEX_POINT ( 'NONE', #11645 ) ;
#13583 = EDGE_CURVE ( 'NONE', #11765, #5753, #2199, .T. ) ;
#13584 = CARTESIAN_POINT ( 'NONE',  ( 0.000000000000000000, 0.000000000000000000, -35.00000000000000000 ) ) ;
#13585 = CIRCLE ( 'NONE', #4962, 24.12539914357697413 ) ;
#13586 = FACE_BOUND ( 'NONE', #228, .T. ) ;
#13587 = PRODUCT_DEFINITION_CONTEXT ( 'detailed design', #9069, 'design' ) ;
#13588 = CYLINDRICAL_SURFACE ( 'NONE', #13420, 8.265000000000021885 ) ;
#13589 = DIRECTION ( 'NONE',  ( -1.000000000000000000, 0.000000000000000000, 0.000000000000000000 ) ) ;
#13590 = EDGE_CURVE ( 'NONE', #15630, #2502, #13699, .T. ) ;
#13591 = DIRECTION ( 'NONE',  ( 1.000000000000000000, 0.000000000000000000, 0.000000000000000000 ) ) ;
#13592 = ORIENTED_EDGE ( 'NONE', *, *, #10073, .T. ) ;
#13593 = CARTESIAN_POINT ( 'NONE',  ( 14.19790265903627180, 9.644882309621939598, 32.00000000000000000 ) ) ;
#13594 = EDGE_CURVE ( 'NONE', #17943, #6326, #7291, .T. ) ;
#13595 = CARTESIAN_POINT ( 'NONE',  ( -3.270778111535288080, 3.632567103900569361, -12.46874999795161543 ) ) ;
#13596 = ORIENTED_EDGE ( 'NONE', *, *, #2197, .T. ) ;
#13597 = CARTESIAN_POINT ( 'NONE',  ( 14.31249999590322552, -5.207209108562836697, 2.318398865532038666 ) ) ;
#13598 = DIRECTION ( 'NONE',  ( -1.000000000000000000, -0.000000000000000000, -0.000000000000000000 ) ) ;
#13599 = AXIS2_PLACEMENT_3D ( 'NONE', #9355, #15754, #15458 ) ;
#13600 = VECTOR ( 'NONE', #8378, 1000.000000000000000 ) ;
#13601 = CARTESIAN_POINT ( 'NONE',  ( 2.255998204157473097, -17.85806462366060288, -35.00000000000000000 ) ) ;
#13602 = CARTESIAN_POINT ( 'NONE',  ( 8.000000000000005329, 5.668774803599156975, 0.5958122406256382009 ) ) ;
#13603 = EDGE_CURVE ( 'NONE', #5154, #7112, #5068, .T. ) ;
#13604 = B_SPLINE_CURVE_WITH_KNOTS ( 'NONE', 3,
 ( #921, #7000, #19615, #4212 ),
 .UNSPECIFIED., .F., .F.,
 ( 4, 4 ),
 ( 1.981826382900849143E-07, 0.0006887856082032012620 ),
 .UNSPECIFIED. ) ;
#13605 = ORIENTED_EDGE ( 'NONE', *, *, #17234, .T. ) ;
#13606 = CARTESIAN_POINT ( 'NONE',  ( 6.000000000000005329, 4.936344801571308061, -2.849999999999988987 ) ) ;
#13607 = DIRECTION ( 'NONE',  ( 0.000000000000000000, 0.000000000000000000, 1.000000000000000000 ) ) ;
#13608 = CARTESIAN_POINT ( 'NONE',  ( 0.02436607992775934733, -21.30679549418640306, 12.59161484032904887 ) ) ;
#13609 = ORIENTED_EDGE ( 'NONE', *, *, #13125, .F. ) ;
#13610 = CARTESIAN_POINT ( 'NONE',  ( 12.31249999590322552, -2.849999999999954792, -4.936344801571327601 ) ) ;
#13611 = CARTESIAN_POINT ( 'NONE',  ( 13.96874999795161365, -4.780397808154265960, 1.280903732194421663 ) ) ;
#13612 = EDGE_CURVE ( 'NONE', #17046, #1899, #9611, .T. ) ;
#13613 = CARTESIAN_POINT ( 'NONE',  ( 6.468749997951615427, -3.413342815706642518E-14, 4.888101187500000222 ) ) ;
#13614 = CARTESIAN_POINT ( 'NONE',  ( 6.843749997951615427, 0.000000000000000000, -4.888101187500000222 ) ) ;
#13615 = DIRECTION ( 'NONE',  ( 1.000000000000000000, 0.000000000000000000, 0.000000000000000000 ) ) ;
#13616 = VECTOR ( 'NONE', #2403, 1000.000000000000000 ) ;
#13617 = CARTESIAN_POINT ( 'NONE',  ( -17.68117051311639898, -3.372863662543042818, -32.00000000000000000 ) ) ;
#13618 = AXIS2_PLACEMENT_3D ( 'NONE', #1420, #15025, #1518 ) ;
#13619 = ORIENTED_EDGE ( 'NONE', *, *, #19413, .T. ) ;
#13620 = CARTESIAN_POINT ( 'NONE',  ( -4.861323657744403448, 0.5109457054262118714, -13.46874999795161543 ) ) ;
#13621 = CARTESIAN_POINT ( 'NONE',  ( 2.000000000000000000, -2.000000000000001776, 41.99999999999999289 ) ) ;
#13622 = ORIENTED_EDGE ( 'NONE', *, *, #84, .F. ) ;
#13623 = EDGE_CURVE ( 'NONE', #6438, #4912, #14029, .T. ) ;
#13624 = FACE_OUTER_BOUND ( 'NONE', #9181, .T. ) ;
#13625 = DIRECTION ( 'NONE',  ( -1.000000000000000000, -0.000000000000000000, -0.000000000000000000 ) ) ;
#13626 = EDGE_LOOP ( 'NONE', ( #8240, #4968, #9089, #1935 ) ) ;
#13627 = AXIS2_PLACEMENT_3D ( 'NONE', #10607, #1502, #13400 ) ;
#13628 = CARTESIAN_POINT ( 'NONE',  ( 3.846120219227944670, 3.114526743279255161, -10.96874999795161720 ) ) ;
#13629 = DIRECTION ( 'NONE',  ( 0.000000000000000000, 0.000000000000000000, 1.000000000000000000 ) ) ;
#13630 = CARTESIAN_POINT ( 'NONE',  ( -9.000000000000000000, 1.102182119232617714E-15, -28.99999999999999645 ) ) ;
#13631 = CIRCLE ( 'NONE', #11392, 2.524999999999995914 ) ;
#13632 = ORIENTED_EDGE ( 'NONE', *, *, #5649, .F. ) ;
#13633 = DIRECTION ( 'NONE',  ( 0.000000000000000000, 0.000000000000000000, 1.000000000000000000 ) ) ;
#13634 = VERTEX_POINT ( 'NONE', #8097 ) ;
#13635 = LINE ( 'NONE', #15243, #14928 ) ;
#13636 = ORIENTED_EDGE ( 'NONE', *, *, #6299, .T. ) ;
#13637 = CARTESIAN_POINT ( 'NONE',  ( -6.626241948324210540, -16.73597674598852336, -35.00000000000000000 ) ) ;
#13638 = DIRECTION ( 'NONE',  ( 1.000000000000000000, 0.000000000000000000, 0.000000000000000000 ) ) ;
#13639 = DIRECTION ( 'NONE',  ( 1.000000000000000000, 0.000000000000000000, 0.000000000000000000 ) ) ;
#13640 = CARTESIAN_POINT ( 'NONE',  ( 10.46874999795161720, -3.632567103900500971, -3.270778111535363131 ) ) ;
#13641 = B_SPLINE_CURVE_WITH_KNOTS ( 'NONE', 3,
 ( #7045, #11384, #6856, #13178 ),
 .UNSPECIFIED., .F., .F.,
 ( 4, 4 ),
 ( 0.005258139959819249469, 0.005948405594583416715 ),
 .UNSPECIFIED. ) ;
#13642 = CARTESIAN_POINT ( 'NONE',  ( 1.749999999999998002, 4.147968289691672084, -27.76164181293047406 ) ) ;
#13643 = VERTEX_POINT ( 'NONE', #14207 ) ;
#13644 = LINE ( 'NONE', #7319, #7097 ) ;
#13645 = CIRCLE ( 'NONE', #11725, 1.000000000000002442 ) ;
#13646 = AXIS2_PLACEMENT_3D ( 'NONE', #12538, #11033, #18830 ) ;
#13647 = PRESENTATION_STYLE_ASSIGNMENT (( #7525 ) ) ;
#13648 = ORIENTED_EDGE ( 'NONE', *, *, #3779, .F. ) ;
#13649 = EDGE_CURVE ( 'NONE', #479, #2446, #13075, .T. ) ;
#13650 = CARTESIAN_POINT ( 'NONE',  ( 0.000000000000000000, 0.000000000000000000, 0.000000000000000000 ) ) ;
#13651 = CARTESIAN_POINT ( 'NONE',  ( 0.02436607992775978102, 16.37294372382885044, -18.55949924794875017 ) ) ;
#13652 = ORIENTED_EDGE ( 'NONE', *, *, #858, .F. ) ;
#13653 = LINE ( 'NONE', #7225, #8965 ) ;
#13654 = CARTESIAN_POINT ( 'NONE',  ( 2.318398865532038666, -5.207209108562836697, -13.00000000000000533 ) ) ;
#13655 = CARTESIAN_POINT ( 'NONE',  ( 2.604434283110813819, -22.53097606932974983, -12.84444904262050002 ) ) ;
#13656 = ORIENTED_EDGE ( 'NONE', *, *, #4205, .F. ) ;
#13657 = CARTESIAN_POINT ( 'NONE',  ( -7.688810570594222860E-14, -5.456611084822025504, 23.69897269326675016 ) ) ;
#13658 = AXIS2_PLACEMENT_3D ( 'NONE', #14818, #10515, #12211 ) ;
#13659 = VERTEX_POINT ( 'NONE', #9039 ) ;
#13660 = DIRECTION ( 'NONE',  ( 1.000000000000000000, 6.419766481290788001E-33, 4.121340167430470643E-65 ) ) ;
#13661 = CARTESIAN_POINT ( 'NONE',  ( 2.601776091974071115, -5.251266773802197640, -25.40949241676359094 ) ) ;
#13662 = EDGE_CURVE ( 'NONE', #1899, #13431, #19445, .T. ) ;
#13663 = AXIS2_PLACEMENT_3D ( 'NONE', #11060, #17168, #2251 ) ;
#13664 = PRESENTATION_STYLE_ASSIGNMENT (( #7646 ) ) ;
#13665 = ORIENTED_EDGE ( 'NONE', *, *, #19384, .T. ) ;
#13666 = VERTEX_POINT ( 'NONE', #10643 ) ;
#13667 = CARTESIAN_POINT ( 'NONE',  ( 0.02436607992776064838, 12.59161484032912171, 21.30679549418635688 ) ) ;
#13668 = CARTESIAN_POINT ( 'NONE',  ( 7.343749997951615427, 0.7741991708318887166, -4.888101187500000222 ) ) ;
#13669 = ORIENTED_EDGE ( 'NONE', *, *, #4824, .T. ) ;
#13670 = CARTESIAN_POINT ( 'NONE',  ( 5.000000000000000000, 0.000000000000000000, 37.99999999999999289 ) ) ;
#13671 = EDGE_CURVE ( 'NONE', #10924, #15369, #12045, .T. ) ;
#13672 = EDGE_LOOP ( 'NONE', ( #6835, #6261 ) ) ;
#13673 = DIRECTION ( 'NONE',  ( -1.000000000000000000, -0.000000000000000000, -0.000000000000000000 ) ) ;
#13674 = AXIS2_PLACEMENT_3D ( 'NONE', #5966, #19383, #12090 ) ;
#13675 = ORIENTED_EDGE ( 'NONE', *, *, #19158, .F. ) ;
#13676 = VECTOR ( 'NONE', #6385, 1000.000000000000000 ) ;
#13677 = DIRECTION ( 'NONE',  ( -1.000000000000000000, -0.000000000000000000, -0.000000000000000000 ) ) ;
#13678 = CARTESIAN_POINT ( 'NONE',  ( 9.843749997951615427, 3.954556930911862000, -2.873153789725825469 ) ) ;
#13679 = DIRECTION ( 'NONE',  ( 1.000000000000000000, 6.419766481290786633E-33, -0.000000000000000000 ) ) ;
#13680 = ORIENTED_EDGE ( 'NONE', *, *, #14395, .F. ) ;
#13681 = CARTESIAN_POINT ( 'NONE',  ( 0.006974771092476448643, 22.53337530003417655, -9.686319561460717154 ) ) ;
#13682 =( NAMED_UNIT ( * ) PLANE_ANGLE_UNIT ( ) SI_UNIT ( $, .RADIAN. ) );
#13683 = CARTESIAN_POINT ( 'NONE',  ( 2.789999999999999147, 15.74360496233381390, 18.28042085475283685 ) ) ;
#13684 = EDGE_CURVE ( 'NONE', #2446, #2766, #15305, .T. ) ;
#13685 = VERTEX_POINT ( 'NONE', #7994 ) ;
#13686 = LINE ( 'NONE', #4184, #15280 ) ;
#13687 = CIRCLE ( 'NONE', #7605, 4.000000000000000000 ) ;
#13688 = FACE_BOUND ( 'NONE', #16480, .T. ) ;
#13689 = CARTESIAN_POINT ( 'NONE',  ( 2.789999999999999147, -23.48180575137734039, 5.535312321042630934 ) ) ;
#13690 = CARTESIAN_POINT ( 'NONE',  ( 12.32184790671639618, 13.12143529358541016, -32.00000000000000000 ) ) ;
#13691 = CARTESIAN_POINT ( 'NONE',  ( 13.00000000000000178, 4.568735188514060575, 1.737869959597756697 ) ) ;
#13692 = EDGE_LOOP ( 'NONE', ( #6497, #5037, #3373, #8787, #18256, #18843, #9937 ) ) ;
#13693 = CARTESIAN_POINT ( 'NONE',  ( 2.000000000000001776, 9.674709713264090115E-16, 7.800000000000000711 ) ) ;
#13694 = CARTESIAN_POINT ( 'NONE',  ( 2.789999999999999591, -24.22479935914660487, 2.133490293296927742 ) ) ;
#13695 = ORIENTED_EDGE ( 'NONE', *, *, #2480, .F. ) ;
#13696 = CARTESIAN_POINT ( 'NONE',  ( 14.19790265903627180, 9.644882309621939598, -35.00000000000000000 ) ) ;
#13697 = ADVANCED_FACE ( 'NONE', ( #15247, #18146 ), #14104, .F. ) ;
#13698 = CARTESIAN_POINT ( 'NONE',  ( -5.207209108562804722, 2.318398865532109276, -15.31249999590322552 ) ) ;
#13699 = CIRCLE ( 'NONE', #2836, 3.968750000000000000 ) ;
#13700 = CARTESIAN_POINT ( 'NONE',  ( 2.765633920072233742, -24.15498966839966855, 5.391175441198523544 ) ) ;
#13701 = EDGE_CURVE ( 'NONE', #19705, #14268, #3501, .T. ) ;
#13702 = EDGE_LOOP ( 'NONE', ( #4640, #14613 ) ) ;
#13703 = DIRECTION ( 'NONE',  ( 0.000000000000000000, 0.000000000000000000, 1.000000000000000000 ) ) ;
#13704 = DIRECTION ( 'NONE',  ( 0.000000000000000000, 0.000000000000000000, -1.000000000000000000 ) ) ;
#13705 =( GEOMETRIC_REPRESENTATION_CONTEXT ( 3 ) GLOBAL_UNCERTAINTY_ASSIGNED_CONTEXT ( ( #11202 ) ) GLOBAL_UNIT_ASSIGNED_CONTEXT ( ( #11473, #9887, #13266 ) ) REPRESENTATION_CONTEXT ( 'NONE', 'WORKASPACE' ) );
#13706 = CARTESIAN_POINT ( 'NONE',  ( 12.00000000000000355, 0.000000000000000000, -4.000000000000000000 ) ) ;
#13707 = ORIENTED_EDGE ( 'NONE', *, *, #11530, .T. ) ;
#13708 =( BOUNDED_SURFACE ( )  B_SPLINE_SURFACE ( 1, 2, ( 
 ( #10997, #4894, #6467, #12797, #12895, #2083, #12603, #2182, #17101, #18690, #14194, #11395, #595, #18993, #15695, #1985, #11195 ),
 ( #17295, #3584, #5284, #693, #4988, #11095, #17495, #9504, #3394, #17197, #14295, #9406, #15797, #9708, #8287, #15505, #1791 ) ),
 .UNSPECIFIED., .F., .F., .F. ) 
 B_SPLINE_SURFACE_WITH_KNOTS ( ( 2, 2 ),
 ( 3, 2, 2, 2, 2, 2, 2, 2, 3 ),
 ( 0.000000000000000000, 1.000000000000000000 ),
 ( 0.000000000000000000, 0.05000000000000000278, 0.1000000000000000056, 0.1499999999999999944, 0.2000000000000000111, 0.2500000000000000000, 0.2999999999999999889, 0.3499999999999999778, 0.4000000000000000222 ),
 .UNSPECIFIED. ) 
 GEOMETRIC_REPRESENTATION_ITEM ( )  RATIONAL_B_SPLINE_SURFACE ( (
 ( 1.000000000000000000, 0.9876883405951377704, 1.000000000000000000, 0.9876883405951377704, 1.000000000000000000, 0.9876883405951377704, 1.000000000000000000, 0.9876883405951377704, 1.000000000000000000, 0.9876883405951377704, 1.000000000000000000, 0.9876883405951377704, 1.000000000000000000, 0.9876883405951377704, 1.000000000000000000, 0.9876883405951377704, 1.000000000000000000),
 ( 1.000000000000000000, 0.9876883405951377704, 1.000000000000000000, 0.9876883405951377704, 1.000000000000000000, 0.9876883405951377704, 1.000000000000000000, 0.9876883405951377704, 1.000000000000000000, 0.9876883405951377704, 1.000000000000000000, 0.9876883405951377704, 1.000000000000000000, 0.9876883405951377704, 1.000000000000000000, 0.9876883405951377704, 1.000000000000000000) ) ) 
 REPRESENTATION_ITEM ( '' )  SURFACE ( )  );
#13709 = EDGE_CURVE ( 'NONE', #12361, #10647, #13738, .T. ) ;
#13710 = CARTESIAN_POINT ( 'NONE',  ( 1.999999999999999556, -5.000000000000001776, 37.99999999999999289 ) ) ;
#13711 = FACE_OUTER_BOUND ( 'NONE', #17526, .T. ) ;
#13712 = LINE ( 'NONE', #8913, #1930 ) ;
#13713 = CARTESIAN_POINT ( 'NONE',  ( 12.96874999795161543, 4.409619785863906571, 2.246813503491833508 ) ) ;
#13714 = ORIENTED_EDGE ( 'NONE', *, *, #15753, .T. ) ;
#13715 = CARTESIAN_POINT ( 'NONE',  ( 2.789999999999999147, 20.70663861606272249, 15.04425356660767932 ) ) ;
#13716 = CIRCLE ( 'NONE', #14680, 4.200000000000001954 ) ;
#13717 = CARTESIAN_POINT ( 'NONE',  ( -0.2590123213420975623, 4.942249507334556924, -8.343749997951613651 ) ) ;
#13718 = ORIENTED_EDGE ( 'NONE', *, *, #1247, .T. ) ;
#13719 = CARTESIAN_POINT ( 'NONE',  ( 9.500000000000005329, 0.3020334839683282424, -5.763142191869152775 ) ) ;
#13720 = LINE ( 'NONE', #5907, #2122 ) ;
#13721 = ORIENTED_EDGE ( 'NONE', *, *, #13252, .T. ) ;
#13722 = DIRECTION ( 'NONE',  ( 0.000000000000000000, 0.000000000000000000, 1.000000000000000000 ) ) ;
#13723 = CARTESIAN_POINT ( 'NONE',  ( 0.7741991708318884946, 4.888101187500000222, -12.34374999795161543 ) ) ;
#13724 = CARTESIAN_POINT ( 'NONE',  ( -3.954556930911881096, -2.873153789725797935, -14.84374999795161543 ) ) ;
#13725 = EDGE_LOOP ( 'NONE', ( #9886, #7027, #10834, #17567 ) ) ;
#13726 = CARTESIAN_POINT ( 'NONE',  ( 7.343749997951615427, 4.620319390059830056, -1.773574444220725521 ) ) ;
#13727 = DIRECTION ( 'NONE',  ( 0.000000000000000000, 0.000000000000000000, 1.000000000000000000 ) ) ;
#13728 = EDGE_CURVE ( 'NONE', #4362, #7839, #4999, .T. ) ;
#13729 = VERTEX_POINT ( 'NONE', #6120 ) ;
#13730 = LINE ( 'NONE', #8735, #6692 ) ;
#13731 = ORIENTED_EDGE ( 'NONE', *, *, #7547, .F. ) ;
#13732 = ADVANCED_FACE ( 'NONE', ( #3025 ), #1898, .F. ) ;
#13733 = CARTESIAN_POINT ( 'NONE',  ( 0.02436607992776628623, 24.63872515616082737, -2.336989772644355590 ) ) ;
#13734 = ORIENTED_EDGE ( 'NONE', *, *, #3812, .F. ) ;
#13735 = AXIS2_PLACEMENT_3D ( 'NONE', #6507, #15732, #535 ) ;
#13736 = LINE ( 'NONE', #3126, #17886 ) ;
#13737 = DIRECTION ( 'NONE',  ( -0.000000000000000000, -0.000000000000000000, 1.000000000000000000 ) ) ;
#13738 = LINE ( 'NONE', #18700, #6983 ) ;
#13739 = DIRECTION ( 'NONE',  ( -1.000000000000000000, -0.000000000000000000, -0.000000000000000000 ) ) ;
#13740 = CARTESIAN_POINT ( 'NONE',  ( 10.96874999795161720, 3.114526743279255161, 3.846120219227944670 ) ) ;
#13741 = EDGE_CURVE ( 'NONE', #16293, #16516, #8200, .T. ) ;
#13742 = ORIENTED_EDGE ( 'NONE', *, *, #8652, .F. ) ;
#13743 = CARTESIAN_POINT ( 'NONE',  ( -2.000000000000001776, 0.000000000000000000, 0.000000000000000000 ) ) ;
#13744 = B_SPLINE_CURVE_WITH_KNOTS ( 'NONE', 3,
 ( #17493, #8580, #5375, #5178 ),
 .UNSPECIFIED., .F., .F.,
 ( 4, 4 ),
 ( 0.005342776758202955750, 0.005948405594583417583 ),
 .UNSPECIFIED. ) ;
#13745 = DIRECTION ( 'NONE',  ( -0.000000000000000000, -0.000000000000000000, 1.000000000000000000 ) ) ;
#13746 = EDGE_CURVE ( 'NONE', #6178, #5524, #12931, .T. ) ;
#13747 = ORIENTED_EDGE ( 'NONE', *, *, #3087, .T. ) ;
#13748 = EDGE_CURVE ( 'NONE', #3576, #4109, #3801, .T. ) ;
#13749 = AXIS2_PLACEMENT_3D ( 'NONE', #3122, #12531, #9634 ) ;
#13750 = PLANE ( 'NONE',  #356 ) ;
#13751 = LINE ( 'NONE', #12354, #11924 ) ;
#13752 = ORIENTED_EDGE ( 'NONE', *, *, #15494, .T. ) ;
#13753 = DIRECTION ( 'NONE',  ( 0.000000000000000000, -1.000000000000000000, 0.000000000000000000 ) ) ;
#13754 = CARTESIAN_POINT ( 'NONE',  ( 1.749999999999998002, 12.52377138324259143, -25.12109765559640451 ) ) ;
#13755 = CARTESIAN_POINT ( 'NONE',  ( 2.765633920072235963, 24.63872515616082737, 2.336989772644355146 ) ) ;
#13756 = ORIENTED_EDGE ( 'NONE', *, *, #3812, .T. ) ;
#13757 = CARTESIAN_POINT ( 'NONE',  ( 11.58013454126452579, -14.56230589874905412, -32.00000000000000000 ) ) ;
#13758 = ORIENTED_EDGE ( 'NONE', *, *, #3631, .T. ) ;
#13759 = APPLICATION_PROTOCOL_DEFINITION ( 'draft international standard', 'automotive_design', 1998, #19276 ) ;
#13760 = CARTESIAN_POINT ( 'NONE',  ( 1.749999999999998002, 24.89775460606851354, -12.96210679857759729 ) ) ;
#13761 = ORIENTED_EDGE ( 'NONE', *, *, #4345, .T. ) ;
#13762 = ORIENTED_EDGE ( 'NONE', *, *, #6094, .T. ) ;
#13763 = DIRECTION ( 'NONE',  ( 1.000000000000000000, 0.000000000000000000, 0.000000000000000000 ) ) ;
#13764 = CONICAL_SURFACE ( 'NONE', #19192, 7.937500000000000000, 1.047197551196596521 ) ;
#13765 = ORIENTED_EDGE ( 'NONE', *, *, #13139, .T. ) ;
#13766 = EDGE_CURVE ( 'NONE', #6991, #12580, #19137, .T. ) ;
#13767 = ORIENTED_EDGE ( 'NONE', *, *, #1813, .T. ) ;
#13768 = CARTESIAN_POINT ( 'NONE',  ( -17.68117051311639898, -3.372863662543042818, 32.00000000000000000 ) ) ;
#13769 = ADVANCED_FACE ( 'NONE', ( #9517 ), #9719, .T. ) ;
#13770 = ORIENTED_EDGE ( 'NONE', *, *, #5731, .F. ) ;
#13771 = EDGE_CURVE ( 'NONE', #3453, #11096, #18342, .T. ) ;
#13772 = CIRCLE ( 'NONE', #10906, 8.000000000000000000 ) ;
#13773 = DIRECTION ( 'NONE',  ( 0.000000000000000000, 0.000000000000000000, -1.000000000000000000 ) ) ;
#13774 = CARTESIAN_POINT ( 'NONE',  ( -3.000000000000002665, 7.347880794884119736E-16, -6.000000000000000000 ) ) ;
#13775 = CARTESIAN_POINT ( 'NONE',  ( 0.000000000000000000, 18.28042085475300382, -15.74360496233363804 ) ) ;
#13776 = ORIENTED_EDGE ( 'NONE', *, *, #13594, .F. ) ;
#13777 = ORIENTED_EDGE ( 'NONE', *, *, #7489, .T. ) ;
#13778 = EDGE_CURVE ( 'NONE', #6546, #12760, #17506, .T. ) ;
#13779 = DIRECTION ( 'NONE',  ( -5.011428603230760289E-33, 0.7806247497997995666, 0.6250000000000002220 ) ) ;
#13780 =( LENGTH_UNIT ( ) NAMED_UNIT ( * ) SI_UNIT ( .MILLI., .METRE. ) );
#13781 = CARTESIAN_POINT ( 'NONE',  ( 2.000000000000000000, 7.800000000000000711, 0.000000000000000000 ) ) ;
#13782 = ORIENTED_EDGE ( 'NONE', *, *, #11780, .T. ) ;
#13783 = DIRECTION ( 'NONE',  ( 0.000000000000000000, -1.000000000000000000, 0.000000000000000000 ) ) ;
#13784 = DIRECTION ( 'NONE',  ( 0.000000000000000000, 0.000000000000000000, 1.000000000000000000 ) ) ;
#13785 = DIRECTION ( 'NONE',  ( 1.000000000000000000, 0.000000000000000000, 0.000000000000000000 ) ) ;
#13786 = CYLINDRICAL_SURFACE ( 'NONE', #3259, 1.000000000000000888 ) ;
#13787 = AXIS2_PLACEMENT_3D ( 'NONE', #6033, #13947, #15454 ) ;
#13788 = LINE ( 'NONE', #5679, #2810 ) ;
#13789 = AXIS2_PLACEMENT_3D ( 'NONE', #12325, #1716, #9522 ) ;
#13790 = ORIENTED_EDGE ( 'NONE', *, *, #14476, .F. ) ;
#13791 = CIRCLE ( 'NONE', #11861, 4.762500000000000178 ) ;
#13792 = DIRECTION ( 'NONE',  ( 1.000000000000000000, 0.000000000000000000, 0.000000000000000000 ) ) ;
#13793 = ORIENTED_EDGE ( 'NONE', *, *, #18151, .T. ) ;
#13794 = CARTESIAN_POINT ( 'NONE',  ( 8.000000000000005329, -2.318398865532001363, -5.207209108562852684 ) ) ;
#13795 = EDGE_CURVE ( 'NONE', #17039, #13382, #5391, .T. ) ;
#13796 = CARTESIAN_POINT ( 'NONE',  ( 0.000000000000000000, 0.000000000000000000, 0.000000000000000000 ) ) ;
#13797 = CARTESIAN_POINT ( 'NONE',  ( 7.468749997951615427, -3.270778111535287191, -3.632567103900569361 ) ) ;
#13798 = CARTESIAN_POINT ( 'NONE',  ( -3.292592168578611034, -7.264456548524809598, -1.328147661294742734E-15 ) ) ;
#13799 = VERTEX_POINT ( 'NONE', #12805 ) ;
#13800 = VECTOR ( 'NONE', #15788, 1000.000000000000114 ) ;
#13801 = DIRECTION ( 'NONE',  ( 0.000000000000000000, 0.000000000000000000, -1.000000000000000000 ) ) ;
#13802 = LINE ( 'NONE', #11908, #7144 ) ;
#13803 = AXIS2_PLACEMENT_3D ( 'NONE', #13715, #15322, #18413 ) ;
#13804 = DIRECTION ( 'NONE',  ( 0.000000000000000000, 0.000000000000000000, -1.000000000000000000 ) ) ;
#13805 = EDGE_LOOP ( 'NONE', ( #15300, #10766, #13828, #12371 ) ) ;
#13806 = DIRECTION ( 'NONE',  ( -1.000000000000000000, -0.000000000000000000, -0.000000000000000000 ) ) ;
#13807 = CARTESIAN_POINT ( 'NONE',  ( 14.34374999795161365, -4.780397808154265960, 1.280903732194421663 ) ) ;
#13808 = DIRECTION ( 'NONE',  ( 0.3826834323650906700, -0.9238795325112864054, 0.000000000000000000 ) ) ;
#13809 = AXIS2_PLACEMENT_3D ( 'NONE', #13980, #17082, #1965 ) ;
#13810 = CARTESIAN_POINT ( 'NONE',  ( -15.00000000000000355, 4.400000000000000355, 0.000000000000000000 ) ) ;
#13811 = ADVANCED_FACE ( 'NONE', ( #704 ), #9626, .F. ) ;
#13812 = EDGE_LOOP ( 'NONE', ( #115, #3364, #17969, #6704, #17432, #14134, #15368, #15456, #3015, #4472, #17141, #19724, #12366, #8177, #14892, #16960, #10653 ) ) ;
#13813 = CARTESIAN_POINT ( 'NONE',  ( 0.000000000000000000, 0.000000000000000000, 0.000000000000000000 ) ) ;
#13814 = DIRECTION ( 'NONE',  ( 0.000000000000000000, 0.000000000000000000, -1.000000000000000000 ) ) ;
#13815 = EDGE_LOOP ( 'NONE', ( #5012, #2499, #4843, #12743 ) ) ;
#13816 = CARTESIAN_POINT ( 'NONE',  ( 8.968749997951611874, -3.499494075959840966, 3.499494075959791672 ) ) ;
#13817 = DIRECTION ( 'NONE',  ( 0.000000000000000000, 0.000000000000000000, 1.000000000000000000 ) ) ;
#13818 = CIRCLE ( 'NONE', #12224, 1.000000000000000888 ) ;
#13819 = VERTEX_POINT ( 'NONE', #8263 ) ;
#13820 = COLOUR_RGB ( '', 0.09019608, 0.27058824, 0.51372549) ;
#13821 = EDGE_CURVE ( 'NONE', #5932, #18318, #13972, .T. ) ;
#13822 = EDGE_CURVE ( 'NONE', #9207, #10667, #3658, .T. ) ;
#13823 = AXIS2_PLACEMENT_3D ( 'NONE', #8594, #10301, #4188 ) ;
#13824 = VECTOR ( 'NONE', #14560, 1000.000000000000000 ) ;
#13825 = CARTESIAN_POINT ( 'NONE',  ( -4.888101187500000222, 0.7741991708318887166, -6.968749997951614539 ) ) ;
#13826 = CARTESIAN_POINT ( 'NONE',  ( 0.000000000000000000, 0.000000000000000000, 6.000000000000000000 ) ) ;
#13827 =( BOUNDED_SURFACE ( )  B_SPLINE_SURFACE ( 1, 2, ( 
 ( #5295, #3596, #15805, #9814, #15907, #18899, #16205, #10104, #11596, #2093, #17408, #13005, #896, #10011, #16109, #803, #14699 ),
 ( #9717, #14514, #2388, #17697, #988, #3993, #3693, #2189, #8502, #13097, #2478, #6679, #604, #8296, #14607, #8592, #6974 ) ),
 .UNSPECIFIED., .F., .F., .F. ) 
 B_SPLINE_SURFACE_WITH_KNOTS ( ( 2, 2 ),
 ( 3, 2, 2, 2, 2, 2, 2, 2, 3 ),
 ( 0.000000000000000000, 1.000000000000000000 ),
 ( 0.000000000000000000, 0.05000000000000000278, 0.1000000000000000056, 0.1499999999999999944, 0.2000000000000000111, 0.2500000000000000000, 0.2999999999999999889, 0.3499999999999999778, 0.4000000000000000222 ),
 .UNSPECIFIED. ) 
 GEOMETRIC_REPRESENTATION_ITEM ( )  RATIONAL_B_SPLINE_SURFACE ( (
 ( 1.000000000000000000, 0.9876883405951377704, 1.000000000000000000, 0.9876883405951377704, 1.000000000000000000, 0.9876883405951377704, 1.000000000000000000, 0.9876883405951377704, 1.000000000000000000, 0.9876883405951377704, 1.000000000000000000, 0.9876883405951377704, 1.000000000000000000, 0.9876883405951377704, 1.000000000000000000, 0.9876883405951377704, 1.000000000000000000),
 ( 1.000000000000000000, 0.9876883405951377704, 1.000000000000000000, 0.9876883405951377704, 1.000000000000000000, 0.9876883405951377704, 1.000000000000000000, 0.9876883405951377704, 1.000000000000000000, 0.9876883405951377704, 1.000000000000000000, 0.9876883405951377704, 1.000000000000000000, 0.9876883405951377704, 1.000000000000000000, 0.9876883405951377704, 1.000000000000000000) ) ) 
 REPRESENTATION_ITEM ( '' )  SURFACE ( )  );
#13828 = ORIENTED_EDGE ( 'NONE', *, *, #11529, .T. ) ;
#13829 = CYLINDRICAL_SURFACE ( 'NONE', #9802, 1.000000000000000888 ) ;
#13830 = CARTESIAN_POINT ( 'NONE',  ( 0.02436607992775761261, 22.71065055754452544, 9.836394144775786330 ) ) ;
#13831 = VERTEX_POINT ( 'NONE', #357 ) ;
#13832 = CARTESIAN_POINT ( 'NONE',  ( 91.50000000000000000, 0.000000000000000000, 0.000000000000000000 ) ) ;
#13833 = ORIENTED_EDGE ( 'NONE', *, *, #19592, .T. ) ;
#13834 = CARTESIAN_POINT ( 'NONE',  ( -41.99999999999999289, -5.000000000000001776, -5.000000000000000000 ) ) ;
#13835 = AXIS2_PLACEMENT_3D ( 'NONE', #11658, #7034, #5259 ) ;
#13836 = ORIENTED_EDGE ( 'NONE', *, *, #4028, .T. ) ;
#13837 = CARTESIAN_POINT ( 'NONE',  ( -17.11901729331276911, 5.562305898749051458, 32.00000000000000000 ) ) ;
#13838 = CARTESIAN_POINT ( 'NONE',  ( -36.00000000000000000, -2.311115933264683024E-31, 0.000000000000000000 ) ) ;
#13839 = CARTESIAN_POINT ( 'NONE',  ( -5.207209108562852684, -2.318398865532001363, -8.000000000000005329 ) ) ;
#13840 = PRODUCT_RELATED_PRODUCT_CATEGORY ( 'part', '', ( #13062 ) ) ;
#13841 = TOROIDAL_SURFACE ( 'NONE', #8400, 7.800000000000000711, 0.1999999999999998723 ) ;
#13842 = CARTESIAN_POINT ( 'NONE',  ( 13.00000000000000000, -1.727010089215899713, -5.432074755721473025 ) ) ;
#13843 = ORIENTED_EDGE ( 'NONE', *, *, #7299, .T. ) ;
#13844 = CARTESIAN_POINT ( 'NONE',  ( 0.000000000000000000, 0.000000000000000000, -22.00000000000000000 ) ) ;
#13845 = CARTESIAN_POINT ( 'NONE',  ( -1.899999999999999023, 0.000000000000000000, -6.760799999999997034 ) ) ;
#13846 = ADVANCED_FACE ( 'NONE', ( #18470 ), #9477, .F. ) ;
#13847 = EDGE_CURVE ( 'NONE', #5711, #14278, #2157, .T. ) ;
#13848 = VECTOR ( 'NONE', #8758, 1000.000000000000000 ) ;
#13849 = EDGE_LOOP ( 'NONE', ( #15495, #1673 ) ) ;
#13850 = CARTESIAN_POINT ( 'NONE',  ( 0.02436607992776455150, -22.71065055754459650, 9.836394144775621129 ) ) ;
#13851 = DIRECTION ( 'NONE',  ( -1.000000000000000000, 0.000000000000000000, 0.000000000000000000 ) ) ;
#13852 = ORIENTED_EDGE ( 'NONE', *, *, #14531, .F. ) ;
#13853 = CARTESIAN_POINT ( 'NONE',  ( 8.500000000000005329, -5.574407415329147852, -1.493657965219562511 ) ) ;
#13854 = CARTESIAN_POINT ( 'NONE',  ( 15.31249999590322552, 5.668774803599165857, -0.5958122406255597081 ) ) ;
#13855 = AXIS2_PLACEMENT_3D ( 'NONE', #7375, #11805, #15309 ) ;
#13856 = ORIENTED_EDGE ( 'NONE', *, *, #9669, .T. ) ;
#13857 = ADVANCED_FACE ( 'NONE', ( #10869 ), #2852, .T. ) ;
#13858 = CARTESIAN_POINT ( 'NONE',  ( -1.800000000000000044, 0.000000000000000000, 0.000000000000000000 ) ) ;
#13859 = ORIENTED_EDGE ( 'NONE', *, *, #12598, .F. ) ;
#13860 = PRODUCT_CONTEXT ( 'NONE', #514, 'mechanical' ) ;
#13861 = LINE ( 'NONE', #153, #8404 ) ;
#13862 = DIRECTION ( 'NONE',  ( -1.000000000000000000, -0.000000000000000000, -0.000000000000000000 ) ) ;
#13863 = ORIENTED_EDGE ( 'NONE', *, *, #11884, .F. ) ;
#13864 = ORIENTED_EDGE ( 'NONE', *, *, #10114, .T. ) ;
#13865 = DIRECTION ( 'NONE',  ( 0.000000000000000000, 0.000000000000000000, 1.000000000000000000 ) ) ;
#13866 = ADVANCED_FACE ( 'NONE', ( #8053 ), #18867, .F. ) ;
#13867 = CARTESIAN_POINT ( 'NONE',  ( 4.780397808154257078, -1.280903732194453637, -14.34374999795161365 ) ) ;
#13869 = EDGE_CURVE ( 'NONE', #4563, #7726, #16924, .T. ) ;
#13868 = EDGE_CURVE ( 'NONE', #18023, #5005, #8162, .T. ) ;
#13870 = ORIENTED_EDGE ( 'NONE', *, *, #5358, .T. ) ;
#13871 = B_SPLINE_CURVE_WITH_KNOTS ( 'NONE', 3,
 ( #2812, #19627, #16836, #10434, #5912, #16733 ),
 .UNSPECIFIED., .F., .F.,
 ( 4, 2, 4 ),
 ( 2.132675795048140432E-07, 0.001878604073277005205, 0.003756994878974505639 ),
 .UNSPECIFIED. ) ;
#13872 = CLOSED_SHELL ( 'NONE', ( #15466, #16422, #6958, #3829, #1749, #7496, #10394, #1904, #8588, #8358, #1486, #10973, #3970, #5760, #14357, #11023, #9550, #13732, #16986, #15337, #11092, #12246, #14413, #14594, #5621, #16437, #3816, #18177, #12565, #10163, #10767, #1311, #1523, #4577, #14292, #7053, #3086, #9954, #4080, #13857, #17662, #9206, #10841, #18110 ) ) ;
#13873 = CARTESIAN_POINT ( 'NONE',  ( 2.789999999999999147, -18.28042085475266276, -15.74360496233401996 ) ) ;
#13874 = AXIS2_PLACEMENT_3D ( 'NONE', #937, #7016, #13140 ) ;
#13875 = ORIENTED_EDGE ( 'NONE', *, *, #16483, .F. ) ;
#13876 = CIRCLE ( 'NONE', #2056, 0.2000000000000005107 ) ;
#13877 = CARTESIAN_POINT ( 'NONE',  ( 7.343749997951615427, 3.846120219227923798, 3.114526743279282694 ) ) ;
#13878 = DIRECTION ( 'NONE',  ( -0.000000000000000000, -0.000000000000000000, 1.000000000000000000 ) ) ;
#13879 = ORIENTED_EDGE ( 'NONE', *, *, #5980, .F. ) ;
#13880 = ORIENTED_EDGE ( 'NONE', *, *, #10690, .T. ) ;
#13881 = CARTESIAN_POINT ( 'NONE',  ( 0.000000000000000000, 22.25075486061751207, -9.324097380959241121 ) ) ;
#13882 =( LENGTH_UNIT ( ) NAMED_UNIT ( * ) SI_UNIT ( .MILLI., .METRE. ) );
#13883 = CIRCLE ( 'NONE', #14538, 24.12539914357697413 ) ;
#13884 = ORIENTED_EDGE ( 'NONE', *, *, #276, .T. ) ;
#13885 = EDGE_LOOP ( 'NONE', ( #13479, #13875, #8511, #14161 ) ) ;
#13886 = CARTESIAN_POINT ( 'NONE',  ( 11.06250000000000000, 0.000000000000000000, 3.797000000000000597 ) ) ;
#13887 = FACE_OUTER_BOUND ( 'NONE', #544, .T. ) ;
#13888 = LINE ( 'NONE', #6265, #8628 ) ;
#13889 = DIRECTION ( 'NONE',  ( 5.011428603230760289E-33, -0.7806247497997995666, 0.6250000000000001110 ) ) ;
#13890 = AXIS2_PLACEMENT_3D ( 'NONE', #13259, #19250, #16259 ) ;
#13891 = CARTESIAN_POINT ( 'NONE',  ( 3.350375938067096548, 4.611396867937201272, -13.00000000000000533 ) ) ;
#13892 = ORIENTED_EDGE ( 'NONE', *, *, #13365, .T. ) ;
#13893 = CARTESIAN_POINT ( 'NONE',  ( 7.343749997951615427, -3.846120219227901149, -3.114526743279308896 ) ) ;
#13894 = CARTESIAN_POINT ( 'NONE',  ( 13.00000000000000000, -4.362347728716193807, -2.206210144330614131 ) ) ;
#13895 = VERTEX_POINT ( 'NONE', #4864 ) ;
#13896 = B_SPLINE_CURVE_WITH_KNOTS ( 'NONE', 3,
 ( #12724, #10925, #15432, #18717 ),
 .UNSPECIFIED., .F., .F.,
 ( 4, 4 ),
 ( 3.059063720795842371E-07, 0.0006888942284914355242 ),
 .UNSPECIFIED. ) ;
#13897 = LINE ( 'NONE', #1883, #10397 ) ;
#13898 = AXIS2_PLACEMENT_3D ( 'NONE', #3192, #12110, #2995 ) ;
#13899 = CARTESIAN_POINT ( 'NONE',  ( 2.765633920072236407, -2.336989772644440855, 24.63872515616082026 ) ) ;
#13900 = DIRECTION ( 'NONE',  ( 1.000000000000000000, 0.000000000000000000, 0.000000000000000000 ) ) ;
#13901 = CARTESIAN_POINT ( 'NONE',  ( 0.07181525068722517668, 2.576941577947404305, 25.22524549359951251 ) ) ;
#13902 = ORIENTED_EDGE ( 'NONE', *, *, #4649, .F. ) ;
#13903 = AXIS2_PLACEMENT_3D ( 'NONE', #10406, #5885, #14807 ) ;
#13904 = CARTESIAN_POINT ( 'NONE',  ( 13.00000000000000533, 4.611396867937201272, 3.350375938067096548 ) ) ;
#13905 = CARTESIAN_POINT ( 'NONE',  ( 9.000000000000001776, 1.102182119232617911E-15, -22.00000000000000000 ) ) ;
#13906 = CARTESIAN_POINT ( 'NONE',  ( 0.000000000000000000, 0.000000000000000000, -33.00000000000000000 ) ) ;
#13907 = VERTEX_POINT ( 'NONE', #14269 ) ;
#13908 = CARTESIAN_POINT ( 'NONE',  ( 1.039999999999996705, -19.67366047555515252, -20.02152543075367319 ) ) ;
#13909 = DIRECTION ( 'NONE',  ( 1.000000000000000000, 0.000000000000000000, 0.000000000000000000 ) ) ;
#13910 = CARTESIAN_POINT ( 'NONE',  ( 12.96874999795161543, 0.2590123213420971182, 4.942249507334556924 ) ) ;
#13911 = EDGE_CURVE ( 'NONE', #9061, #17079, #11660, .T. ) ;
#13912 = FACE_OUTER_BOUND ( 'NONE', #7017, .T. ) ;
#13913 = ORIENTED_EDGE ( 'NONE', *, *, #12482, .T. ) ;
#13914 = CARTESIAN_POINT ( 'NONE',  ( 1.039999999999999147, 12.52377138324259676, -25.12109765559640095 ) ) ;
#13915 = APPLICATION_CONTEXT ( 'automotive_design' ) ;
#13916 = CARTESIAN_POINT ( 'NONE',  ( -15.00000000000000355, -4.400000000000000355, 5.388445916248354013E-16 ) ) ;
#13917 = ORIENTED_EDGE ( 'NONE', *, *, #4420, .F. ) ;
#13918 = CARTESIAN_POINT ( 'NONE',  ( 10.34374999795161543, -4.409619785863921670, 2.246813503491803310 ) ) ;
#13919 = DIRECTION ( 'NONE',  ( 1.000000000000000000, 0.000000000000000000, 0.000000000000000000 ) ) ;
#13920 = AXIS2_PLACEMENT_3D ( 'NONE', #3128, #16947, #7920 ) ;
#13921 = ORIENTED_EDGE ( 'NONE', *, *, #14344, .T. ) ;
#13922 = CIRCLE ( 'NONE', #10739, 4.000000000000000000 ) ;
#13923 = FACE_OUTER_BOUND ( 'NONE', #16428, .T. ) ;
#13924 = ADVANCED_FACE ( 'NONE', ( #14167 ), #470, .T. ) ;
#13925 = CARTESIAN_POINT ( 'NONE',  ( 1.749999999999998002, 24.89775460606832524, 12.96210679857795256 ) ) ;
#13926 = ORIENTED_EDGE ( 'NONE', *, *, #5127, .F. ) ;
#13927 = CARTESIAN_POINT ( 'NONE',  ( 0.000000000000000000, 0.000000000000000000, 0.000000000000000000 ) ) ;
#13928 = CARTESIAN_POINT ( 'NONE',  ( -4.888101187500000222, 0.000000000000000000, -6.468749997951615427 ) ) ;
#13929 = EDGE_LOOP ( 'NONE', ( #17749, #13767 ) ) ;
#13930 = DIRECTION ( 'NONE',  ( 0.000000000000000000, 1.374038396813314756E-15, -1.000000000000000000 ) ) ;
#13931 = VERTEX_POINT ( 'NONE', #5058 ) ;
#13932 = DIRECTION ( 'NONE',  ( -0.000000000000000000, -0.000000000000000000, 1.000000000000000000 ) ) ;
#13933 = AXIS2_PLACEMENT_3D ( 'NONE', #19449, #8857, #5738 ) ;
#13934 = ORIENTED_EDGE ( 'NONE', *, *, #15171, .T. ) ;
#13935 = DIRECTION ( 'NONE',  ( -0.000000000000000000, -0.000000000000000000, 1.000000000000000000 ) ) ;
#13936 = ADVANCED_FACE ( 'NONE', ( #3556 ), #9680, .F. ) ;
#13937 = VECTOR ( 'NONE', #14639, 1000.000000000000000 ) ;
#13938 = CARTESIAN_POINT ( 'NONE',  ( 2.255998204157473097, -17.85806462366060288, 35.00000000000000000 ) ) ;
#13939 = DIRECTION ( 'NONE',  ( -1.000000000000000000, -0.000000000000000000, -0.000000000000000000 ) ) ;
#13940 = CARTESIAN_POINT ( 'NONE',  ( 4.150607464521812062, 2.695436003842704764, -7.968749997951616315 ) ) ;
#13941 = ORIENTED_EDGE ( 'NONE', *, *, #4170, .T. ) ;
#13942 = FACE_OUTER_BOUND ( 'NONE', #17252, .T. ) ;
#13943 = CARTESIAN_POINT ( 'NONE',  ( -17.96448111170888851, 1.130229351527647585, 32.00000000000000000 ) ) ;
#13944 = CONICAL_SURFACE ( 'NONE', #10110, 3.323500000000020993, 0.7853981633974463916 ) ;
#13945 = ORIENTED_EDGE ( 'NONE', *, *, #12879, .T. ) ;
#13946 = AXIS2_PLACEMENT_3D ( 'NONE', #6788, #13015, #2485 ) ;
#13947 = DIRECTION ( 'NONE',  ( -1.000000000000000000, 1.224646799147353207E-16, 0.000000000000000000 ) ) ;
#13948 = EDGE_CURVE ( 'NONE', #13547, #2023, #15000, .T. ) ;
#13949 = DIRECTION ( 'NONE',  ( 0.000000000000000000, 0.000000000000000000, -1.000000000000000000 ) ) ;
#13950 = EDGE_LOOP ( 'NONE', ( #19076, #17029, #10133, #2143, #10286, #5245, #9925, #13756, #6303, #12432, #19670, #1501, #10082, #17941, #5978, #4208, #1517, #4372, #17365, #17441, #17158, #13286, #12574, #1718 ) ) ;
#13951 = CARTESIAN_POINT ( 'NONE',  ( 2.601776144743014108, 10.68696068830440815, -23.64332819722370260 ) ) ;
#13952 = CARTESIAN_POINT ( 'NONE',  ( 13.81249999590322552, 4.840010801796527318, -3.143139765844555900 ) ) ;
#13953 = ORIENTED_EDGE ( 'NONE', *, *, #6711, .F. ) ;
#13954 = DIRECTION ( 'NONE',  ( -0.000000000000000000, -0.000000000000000000, -1.000000000000000000 ) ) ;
#13955 = EDGE_CURVE ( 'NONE', #18092, #3037, #305, .T. ) ;
#13956 = ORIENTED_EDGE ( 'NONE', *, *, #14016, .T. ) ;
#13957 = APPLICATION_PROTOCOL_DEFINITION ( 'draft international standard', 'automotive_design', 1998, #16983 ) ;
#13958 = CARTESIAN_POINT ( 'NONE',  ( -41.99999999999999289, 1.999999999999997335, -5.000000000000000000 ) ) ;
#13959 = CARTESIAN_POINT ( 'NONE',  ( 10.46874999795161720, 3.632567103900523620, 3.270778111535338262 ) ) ;
#13960 = ORIENTED_EDGE ( 'NONE', *, *, #2245, .T. ) ;
#13961 = ORIENTED_EDGE ( 'NONE', *, *, #9048, .F. ) ;
#13962 = EDGE_CURVE ( 'NONE', #1328, #283, #12677, .T. ) ;
#13963 = DIRECTION ( 'NONE',  ( 1.000000000000000000, 0.000000000000000000, 0.000000000000000000 ) ) ;
#13964 = CARTESIAN_POINT ( 'NONE',  ( 4.233219804643887585, 2.444050593749991229, -11.84374999795161365 ) ) ;
#13965 = VECTOR ( 'NONE', #12637, 1000.000000000000000 ) ;
#13966 = ORIENTED_EDGE ( 'NONE', *, *, #4561, .T. ) ;
#13967 = CARTESIAN_POINT ( 'NONE',  ( -15.19790265903627180, 9.644882309621941374, 35.00000000000000000 ) ) ;
#13968 = ADVANCED_FACE ( 'NONE', ( #16174 ), #4153, .F. ) ;
#13969 = ORIENTED_EDGE ( 'NONE', *, *, #18687, .F. ) ;
#13970 = AXIS2_PLACEMENT_3D ( 'NONE', #7158, #7059, #2768 ) ;
#13971 = ADVANCED_FACE ( 'NONE', ( #6845 ), #16359, .T. ) ;
#13972 = LINE ( 'NONE', #6742, #626 ) ;
#13973 = AXIS2_PLACEMENT_3D ( 'NONE', #6242, #7650, #2954 ) ;
#13974 = EDGE_CURVE ( 'NONE', #11016, #6403, #19351, .T. ) ;
#13975 = CARTESIAN_POINT ( 'NONE',  ( -2.255998204157477538, -17.85806462366060288, -32.00000000000000000 ) ) ;
#13976 = DIRECTION ( 'NONE',  ( -0.000000000000000000, 0.000000000000000000, 1.000000000000000000 ) ) ;
#13977 = VERTEX_POINT ( 'NONE', #13262 ) ;
#13978 = DIRECTION ( 'NONE',  ( -0.000000000000000000, -0.000000000000000000, 1.000000000000000000 ) ) ;
#13979 =( NAMED_UNIT ( * ) SI_UNIT ( $, .STERADIAN. ) SOLID_ANGLE_UNIT ( ) );
#13980 = CARTESIAN_POINT ( 'NONE',  ( 2.789999999999999147, -24.44424927289185590, -0.2301004812060095106 ) ) ;
#13981 = ORIENTED_EDGE ( 'NONE', *, *, #7711, .F. ) ;
#13982 = ORIENTED_EDGE ( 'NONE', *, *, #216, .F. ) ;
#13983 = CARTESIAN_POINT ( 'NONE',  ( 2.031033465052724196, 4.828387785248403397, -27.14933624560903525 ) ) ;
#13984 = CARTESIAN_POINT ( 'NONE',  ( 2.068159791354145849, -5.387740456496247887, -7.812499995903224637 ) ) ;
#13985 = CARTESIAN_POINT ( 'NONE',  ( -5.700000000000001066, 0.2987243419133610023, -12.83455515208546238 ) ) ;
#13986 = CARTESIAN_POINT ( 'NONE',  ( 16.19790265903627358, 9.644882309621939598, -35.00000000000000000 ) ) ;
#13987 = AXIS2_PLACEMENT_3D ( 'NONE', #7822, #13932, #17037 ) ;
#13988 = CARTESIAN_POINT ( 'NONE',  ( -3.270778111535288080, 3.632567103900569361, -12.84374999795161543 ) ) ;
#13989 = AXIS2_PLACEMENT_3D ( 'NONE', #14541, #925, #13127 ) ;
#13990 = VERTEX_POINT ( 'NONE', #770 ) ;
#13991 = ADVANCED_FACE ( 'NONE', ( #17470 ), #16074, .F. ) ;
#13992 = CARTESIAN_POINT ( 'NONE',  ( 2.031033465052725084, -27.14933624560904946, -4.828387785248313691 ) ) ;
#13993 = ADVANCED_FACE ( 'NONE', ( #16265 ), #2357, .T. ) ;
#13994 = LINE ( 'NONE', #18884, #9485 ) ;
#13995 = ORIENTED_EDGE ( 'NONE', *, *, #17258, .F. ) ;
#13996 = CARTESIAN_POINT ( 'NONE',  ( -7.728448779411724935E-14, -2.133839912090635949, -24.22524813288764989 ) ) ;
#13997 = CARTESIAN_POINT ( 'NONE',  ( 10.34374999795161543, -4.150607464521772094, -2.695436003842760275 ) ) ;
#13998 = EDGE_CURVE ( 'NONE', #12385, #8529, #14861, .T. ) ;
#13999 = DIRECTION ( 'NONE',  ( -1.000000000000000000, 0.000000000000000000, 0.000000000000000000 ) ) ;
#14000 = CARTESIAN_POINT ( 'NONE',  ( 0.000000000000000000, -23.48180575137727288, -5.535312321042949790 ) ) ;
#14001 = ORIENTED_EDGE ( 'NONE', *, *, #7731, .T. ) ;
#14002 = CIRCLE ( 'NONE', #583, 28.06981291497571007 ) ;
#14003 = DIRECTION ( 'NONE',  ( 0.000000000000000000, 0.000000000000000000, 1.000000000000000000 ) ) ;
#14004 = DIRECTION ( 'NONE',  ( -1.000000000000000000, -0.000000000000000000, -0.000000000000000000 ) ) ;
#14005 = AXIS2_PLACEMENT_3D ( 'NONE', #11995, #8794, #7267 ) ;
#14006 = FACE_OUTER_BOUND ( 'NONE', #14683, .T. ) ;
#14007 = EDGE_LOOP ( 'NONE', ( #6984, #4330, #13073, #10818 ) ) ;
#14008 = CARTESIAN_POINT ( 'NONE',  ( 2.783025342027735327, -5.408388659523925668, -23.92335783895643075 ) ) ;
#14009 = CARTESIAN_POINT ( 'NONE',  ( 11.00000000000000711, 2.849999999999989431, 4.936344801571308061 ) ) ;
#14010 = CARTESIAN_POINT ( 'NONE',  ( 13.00000000000000000, -3.840809689102975710, 4.211671987713753396 ) ) ;
#14011 = ORIENTED_EDGE ( 'NONE', *, *, #18969, .T. ) ;
#14012 = FACE_OUTER_BOUND ( 'NONE', #8488, .T. ) ;
#14013 = CARTESIAN_POINT ( 'NONE',  ( -4.409619785863906571, 2.246813503491833508, -8.343749997951613651 ) ) ;
#14014 = ORIENTED_EDGE ( 'NONE', *, *, #18131, .F. ) ;
#14015 = CARTESIAN_POINT ( 'NONE',  ( 10.96874999795161720, -4.888101187500005551, 0.7741991708318548548 ) ) ;
#14016 = EDGE_CURVE ( 'NONE', #19358, #19556, #13716, .T. ) ;
#14017 = DIRECTION ( 'NONE',  ( 0.000000000000000000, 0.000000000000000000, -1.000000000000000000 ) ) ;
#14018 = CIRCLE ( 'NONE', #7275, 1.000000000000002665 ) ;
#14019 = EDGE_LOOP ( 'NONE', ( #15685, #3061, #17328, #14118 ) ) ;
#14020 = EDGE_CURVE ( 'NONE', #2162, #3518, #17, .T. ) ;
#14021 = CARTESIAN_POINT ( 'NONE',  ( -2.000000000000001776, 6.368163355566236381E-16, 5.200000000000000178 ) ) ;
#14022 = FACE_OUTER_BOUND ( 'NONE', #6843, .T. ) ;
#14023 = ORIENTED_EDGE ( 'NONE', *, *, #17702, .F. ) ;
#14024 = DIRECTION ( 'NONE',  ( 0.000000000000000000, 0.000000000000000000, 1.000000000000000000 ) ) ;
#14025 = CARTESIAN_POINT ( 'NONE',  ( 1.886022603841296608, 8.263794135966437014E-16, 6.735000000000022524 ) ) ;
#14026 = VERTEX_POINT ( 'NONE', #8653 ) ;
#14027 = DIRECTION ( 'NONE',  ( 0.000000000000000000, -0.8090169943749488946, 0.5877852522924711387 ) ) ;
#14028 = ORIENTED_EDGE ( 'NONE', *, *, #5596, .F. ) ;
#14030 = CARTESIAN_POINT ( 'NONE',  ( 5.387740456496221242, -2.068159791354220900, -11.81249999590322552 ) ) ;
#14029 = CIRCLE ( 'NONE', #9236, 1.000000000000002665 ) ;
#14031 = ORIENTED_EDGE ( 'NONE', *, *, #19071, .F. ) ;
#14032 = EDGE_CURVE ( 'NONE', #15581, #6896, #16258, .T. ) ;
#14033 = CARTESIAN_POINT ( 'NONE',  ( 2.789999999999999147, 15.04425356660790136, -18.18163861606255338 ) ) ;
#14034 = CARTESIAN_POINT ( 'NONE',  ( 4.150607464521812062, 2.695436003842704764, -7.968749997951616315 ) ) ;
#14035 = CARTESIAN_POINT ( 'NONE',  ( 4.781284448697187273, -1.016293382781444654, -10.84374999795161543 ) ) ;
#14036 = ORIENTED_EDGE ( 'NONE', *, *, #15930, .F. ) ;
#14037 = DIRECTION ( 'NONE',  ( -0.4999999999999980016, 0.7500000000000048850, -0.4330127018922129700 ) ) ;
#14038 = DIRECTION ( 'NONE',  ( 1.000000000000000000, 0.000000000000000000, 0.000000000000000000 ) ) ;
#14039 = VECTOR ( 'NONE', #9655, 1000.000000000000114 ) ;
#14040 = ORIENTED_EDGE ( 'NONE', *, *, #4328, .T. ) ;
#14041 = ADVANCED_FACE ( 'NONE', ( #19159 ), #11486, .T. ) ;
#14042 = DIRECTION ( 'NONE',  ( 0.000000000000000000, 0.000000000000000000, 1.000000000000000000 ) ) ;
#14043 = CARTESIAN_POINT ( 'NONE',  ( -6.929096493834647319, 2.870125742738179664, 0.000000000000000000 ) ) ;
#14044 = ORIENTED_EDGE ( 'NONE', *, *, #16013, .T. ) ;
#14046 = CARTESIAN_POINT ( 'NONE',  ( -90.00000000000000000, 8.247996192257451316E-16, 6.735000000000022524 ) ) ;
#14045 = AXIS2_PLACEMENT_3D ( 'NONE', #13561, #1459, #14965 ) ;
#14047 = VERTEX_POINT ( 'NONE', #13162 ) ;
#14048 = CARTESIAN_POINT ( 'NONE',  ( 7.937500000000000000, 4.582717761692648217, -6.527800000000000047 ) ) ;
#14049 = EDGE_LOOP ( 'NONE', ( #3125, #2514, #18141, #8193, #18439, #919 ) ) ;
#14050 = APPLICATION_PROTOCOL_DEFINITION ( 'draft international standard', 'automotive_design', 1998, #12515 ) ;
#14051 = CARTESIAN_POINT ( 'NONE',  ( 2.031033467310408014, 12.98167595241057626, -24.32849926382737138 ) ) ;
#14052 = FACE_OUTER_BOUND ( 'NONE', #14473, .T. ) ;
#14053 = ORIENTED_EDGE ( 'NONE', *, *, #13098, .T. ) ;
#14054 = VERTEX_POINT ( 'NONE', #5258 ) ;
#14055 = DIRECTION ( 'NONE',  ( 0.000000000000000000, 0.000000000000000000, 1.000000000000000000 ) ) ;
#14056 = CARTESIAN_POINT ( 'NONE',  ( 9.468749997951615427, 0.5109457054261445919, 4.861323657744411442 ) ) ;
#14057 = VERTEX_POINT ( 'NONE', #12971 ) ;
#14058 = EDGE_CURVE ( 'NONE', #6283, #14247, #5547, .T. ) ;
#14059 = EDGE_CURVE ( 'NONE', #11508, #1430, #17564, .T. ) ;
#14060 = VECTOR ( 'NONE', #15440, 1000.000000000000000 ) ;
#14061 = VECTOR ( 'NONE', #915, 1000.000000000000000 ) ;
#14062 = ORIENTED_EDGE ( 'NONE', *, *, #13590, .F. ) ;
#14063 = ADVANCED_FACE ( 'NONE', ( #16958 ), #15752, .F. ) ;
#14064 = DIRECTION ( 'NONE',  ( -1.000000000000000000, 0.000000000000000000, -0.000000000000000000 ) ) ;
#14065 = DIRECTION ( 'NONE',  ( 0.000000000000000000, 0.000000000000000000, -1.000000000000000000 ) ) ;
#14066 = CARTESIAN_POINT ( 'NONE',  ( 0.000000000000000000, 0.000000000000000000, -32.00000000000000000 ) ) ;
#14067 = EDGE_LOOP ( 'NONE', ( #3213, #10918, #16562, #2000 ) ) ;
#14068 = AXIS2_PLACEMENT_3D ( 'NONE', #11499, #13198, #17303 ) ;
#14069 = CARTESIAN_POINT ( 'NONE',  ( 18.11901729331276911, 5.562305898749055011, -32.00000000000000000 ) ) ;
#14070 =( LENGTH_UNIT ( ) NAMED_UNIT ( * ) SI_UNIT ( .MILLI., .METRE. ) );
#14071 = PRESENTATION_LAYER_ASSIGNMENT (  '', '', ( #15990 ) ) ;
#14072 = FACE_OUTER_BOUND ( 'NONE', #15827, .T. ) ;
#14073 = ORIENTED_EDGE ( 'NONE', *, *, #18988, .F. ) ;
#14074 = ORIENTED_EDGE ( 'NONE', *, *, #5985, .T. ) ;
#14075 = DIRECTION ( 'NONE',  ( 1.000000000000000000, 1.224646799147353207E-16, 0.000000000000000000 ) ) ;
#14076 = CARTESIAN_POINT ( 'NONE',  ( -3.814044456245531567, -4.235925505221111997, -11.31249999590322375 ) ) ;
#14077 = DIRECTION ( 'NONE',  ( 0.4330127018922130255, -0.7500000000000049960, 0.4999999999999980571 ) ) ;
#14078 = CARTESIAN_POINT ( 'NONE',  ( 13.00000000000000178, 3.908719486245998187, -2.935207862669990231 ) ) ;
#14079 = CARTESIAN_POINT ( 'NONE',  ( -3.814044456245444081, 4.235925505221192822, -13.31249999590322730 ) ) ;
#14080 = ORIENTED_EDGE ( 'NONE', *, *, #17655, .F. ) ;
#14081 = CARTESIAN_POINT ( 'NONE',  ( -0.2436698586202288019, 0.000000000000000000, 0.000000000000000000 ) ) ;
#14082 = FACE_OUTER_BOUND ( 'NONE', #16579, .T. ) ;
#14083 = ORIENTED_EDGE ( 'NONE', *, *, #17501, .T. ) ;
#14084 = CARTESIAN_POINT ( 'NONE',  ( 2.000000000000000000, 1.999999999999998224, 37.99999999999999289 ) ) ;
#14085 = EDGE_CURVE ( 'NONE', #15252, #13330, #16274, .T. ) ;
#14086 = EDGE_CURVE ( 'NONE', #5856, #5054, #6419, .T. ) ;
#14087 = CARTESIAN_POINT ( 'NONE',  ( -11.00000000000000355, -3.278623949159158446, -2.625000000000002220 ) ) ;
#14088 = CARTESIAN_POINT ( 'NONE',  ( 13.00000000000000000, -4.125339889944092953, 2.622041954598548941 ) ) ;
#14089 = CARTESIAN_POINT ( 'NONE',  ( 1.039999999999996483, 4.147968289691283950, 27.76164181293052735 ) ) ;
#14090 = LINE ( 'NONE', #9601, #16800 ) ;
#14091 = EDGE_LOOP ( 'NONE', ( #9201, #15976, #8759, #705 ) ) ;
#14092 = CARTESIAN_POINT ( 'NONE',  ( 11.50000000000000355, 5.699999999999999289, 0.9027913098498566713 ) ) ;
#14093 =( LENGTH_UNIT ( ) NAMED_UNIT ( * ) SI_UNIT ( .MILLI., .METRE. ) );
#14094 = CARTESIAN_POINT ( 'NONE',  ( 13.86923836996420789, -11.47363181547641453, 32.00000000000000000 ) ) ;
#14095 = CARTESIAN_POINT ( 'NONE',  ( -2.849999999999989431, 4.936344801571308061, -7.312499995903225525 ) ) ;
#14096 = ORIENTED_EDGE ( 'NONE', *, *, #7956, .T. ) ;
#14097 = EDGE_CURVE ( 'NONE', #15404, #7834, #9253, .T. ) ;
#14098 = PLANE ( 'NONE',  #260 ) ;
#14099 = CIRCLE ( 'NONE', #2576, 7.174999999999999822 ) ;
#14100 = CYLINDRICAL_SURFACE ( 'NONE', #100, 5.700000000000001954 ) ;
#14101 = AXIS2_PLACEMENT_3D ( 'NONE', #4735, #12545, #18732 ) ;
#14102 = CARTESIAN_POINT ( 'NONE',  ( 6.968749997951614539, 4.620319390059829168, -1.773574444220725077 ) ) ;
#14103 = DIRECTION ( 'NONE',  ( -1.000000000000000000, -0.000000000000000000, -0.000000000000000000 ) ) ;
#14104 = PLANE ( 'NONE',  #14345 ) ;
#14105 = ORIENTED_EDGE ( 'NONE', *, *, #14369, .T. ) ;
#14106 = FACE_OUTER_BOUND ( 'NONE', #17802, .T. ) ;
#14107 = CARTESIAN_POINT ( 'NONE',  ( 2.246813503491833508, 4.409619785863906571, -13.34374999795161365 ) ) ;
#14108 = EDGE_CURVE ( 'NONE', #6632, #15965, #1571, .T. ) ;
#14109 = ORIENTED_EDGE ( 'NONE', *, *, #10170, .T. ) ;
#14110 = CARTESIAN_POINT ( 'NONE',  ( 14.46874999795161720, -2.873153789725797935, -3.954556930911881096 ) ) ;
#14111 = CARTESIAN_POINT ( 'NONE',  ( -34.92499999999994742, 0.000000000000000000, 6.000000000000000000 ) ) ;
#14112 = ORIENTED_EDGE ( 'NONE', *, *, #9080, .T. ) ;
#14113 = AXIS2_PLACEMENT_3D ( 'NONE', #13214, #2204, #11703 ) ;
#14114 = AXIS2_PLACEMENT_3D ( 'NONE', #5776, #19692, #17803 ) ;
#14115 = CIRCLE ( 'NONE', #3248, 24.12539914357697768 ) ;
#14116 = DIRECTION ( 'NONE',  ( 0.000000000000000000, 1.000000000000000000, 0.000000000000000000 ) ) ;
#14117 = DIRECTION ( 'NONE',  ( -1.000000000000000000, 0.000000000000000000, 0.000000000000000000 ) ) ;
#14118 = ORIENTED_EDGE ( 'NONE', *, *, #6129, .F. ) ;
#14119 = DIRECTION ( 'NONE',  ( 0.000000000000000000, 0.000000000000000000, -1.000000000000000000 ) ) ;
#14120 = DIRECTION ( 'NONE',  ( 0.000000000000000000, 0.000000000000000000, 1.000000000000000000 ) ) ;
#14121 = CIRCLE ( 'NONE', #11567, 1.000000000000002665 ) ;
#14122 = EDGE_CURVE ( 'NONE', #10318, #8201, #581, .T. ) ;
#14123 = ORIENTED_EDGE ( 'NONE', *, *, #13911, .T. ) ;
#14124 = CARTESIAN_POINT ( 'NONE',  ( -11.00000000000000355, -4.215373648918918192, 3.375000000000000888 ) ) ;
#14125 = ORIENTED_EDGE ( 'NONE', *, *, #3937, .T. ) ;
#14126 = B_SPLINE_CURVE_WITH_KNOTS ( 'NONE', 3,
 ( #19130, #5515, #18837, #9947 ),
 .UNSPECIFIED., .F., .F.,
 ( 4, 4 ),
 ( 0.005258120783916789796, 0.005948386350302922905 ),
 .UNSPECIFIED. ) ;
#14127 = DIRECTION ( 'NONE',  ( 0.000000000000000000, -0.7806247497997995666, 0.6250000000000002220 ) ) ;
#14128 = VERTEX_POINT ( 'NONE', #11047 ) ;
#14129 = LINE ( 'NONE', #7824, #14060 ) ;
#14130 = LINE ( 'NONE', #15734, #3734 ) ;
#14131 = DIRECTION ( 'NONE',  ( 0.000000000000000000, 0.000000000000000000, 1.000000000000000000 ) ) ;
#14132 = VECTOR ( 'NONE', #1071, 1000.000000000000000 ) ;
#14133 = DIRECTION ( 'NONE',  ( 0.000000000000000000, 0.000000000000000000, 1.000000000000000000 ) ) ;
#14134 = ORIENTED_EDGE ( 'NONE', *, *, #12380, .F. ) ;
#14135 = AXIS2_PLACEMENT_3D ( 'NONE', #2675, #13290, #1090 ) ;
#14136 = CARTESIAN_POINT ( 'NONE',  ( 7.078124996927420476, -4.584782303107616031, 2.647025296874957689 ) ) ;
#14137 = FACE_OUTER_BOUND ( 'NONE', #2822, .T. ) ;
#14138 = B_SPLINE_CURVE_WITH_KNOTS ( 'NONE', 3,
 ( #10722, #13518, #4506, #16833, #19623, #2903 ),
 .UNSPECIFIED., .F., .F.,
 ( 4, 2, 4 ),
 ( 2.132675795046084789E-07, 0.001878604073277003903, 0.003756994878974503470 ),
 .UNSPECIFIED. ) ;
#14139 = EDGE_LOOP ( 'NONE', ( #15927, #18479 ) ) ;
#14140 = PRESENTATION_LAYER_ASSIGNMENT (  '', '', ( #9681 ) ) ;
#14141 = DIRECTION ( 'NONE',  ( -0.000000000000000000, -0.000000000000000000, 1.000000000000000000 ) ) ;
#14142 = CARTESIAN_POINT ( 'NONE',  ( -17.96448111170888851, 1.130229351527647585, 35.00000000000000000 ) ) ;
#14143 = CARTESIAN_POINT ( 'NONE',  ( -1.988169868018624609, -4.465502636338009701, -9.468749997951615427 ) ) ;
#14144 = ORIENTED_EDGE ( 'NONE', *, *, #9426, .F. ) ;
#14145 = AXIS2_PLACEMENT_3D ( 'NONE', #10870, #1865, #11069 ) ;
#14146 = DIRECTION ( 'NONE',  ( 0.000000000000000000, 0.000000000000000000, 1.000000000000000000 ) ) ;
#14147 = DIRECTION ( 'NONE',  ( 1.000000000000000000, 1.224646799147353207E-16, -0.000000000000000000 ) ) ;
#14148 = CIRCLE ( 'NONE', #10594, 7.500000000000000000 ) ;
#14149 = ORIENTED_EDGE ( 'NONE', *, *, #9103, .F. ) ;
#14150 = FACE_OUTER_BOUND ( 'NONE', #5421, .T. ) ;
#14151 = ORIENTED_EDGE ( 'NONE', *, *, #6214, .F. ) ;
#14152 = VECTOR ( 'NONE', #6225, 1000.000000000000000 ) ;
#14153 = PRODUCT_CONTEXT ( 'NONE', #2652, 'mechanical' ) ;
#14154 = DIRECTION ( 'NONE',  ( 0.000000000000000000, 0.000000000000000000, 1.000000000000000000 ) ) ;
#14155 = CARTESIAN_POINT ( 'NONE',  ( 6.968749997951614539, 4.620319390059829168, -1.773574444220725077 ) ) ;
#14156 = ORIENTED_EDGE ( 'NONE', *, *, #5489, .T. ) ;
#14157 = ORIENTED_EDGE ( 'NONE', *, *, #10872, .F. ) ;
#14158 = CARTESIAN_POINT ( 'NONE',  ( 0.02436607992776064838, 5.391175441198615914, 24.15498966839965078 ) ) ;
#14159 = DIRECTION ( 'NONE',  ( 0.000000000000000000, 0.000000000000000000, -1.000000000000000000 ) ) ;
#14160 = EDGE_CURVE ( 'NONE', #11385, #18023, #12274, .T. ) ;
#14161 = ORIENTED_EDGE ( 'NONE', *, *, #2271, .T. ) ;
#14162 = CIRCLE ( 'NONE', #2022, 4.000000000000000000 ) ;
#14163 = CARTESIAN_POINT ( 'NONE',  ( -2.444050593750049849, -4.233219804643852946, -6.843749997951615427 ) ) ;
#14164 = ORIENTED_EDGE ( 'NONE', *, *, #5365, .T. ) ;
#14165 = AXIS2_PLACEMENT_3D ( 'NONE', #18329, #7300, #9127 ) ;
#14166 = CIRCLE ( 'NONE', #4569, 2.524999999999995470 ) ;
#14167 = FACE_OUTER_BOUND ( 'NONE', #4025, .T. ) ;
#14168 = CARTESIAN_POINT ( 'NONE',  ( 8.000000000000000000, 0.000000000000000000, 0.000000000000000000 ) ) ;
#14169 = EDGE_CURVE ( 'NONE', #9243, #13977, #1644, .T. ) ;
#14170 = CARTESIAN_POINT ( 'NONE',  ( 0.02436607992776758727, 24.15498966839963302, 5.391175441198700291 ) ) ;
#14171 = EDGE_LOOP ( 'NONE', ( #3505, #5160, #13636, #3798 ) ) ;
#14172 = CARTESIAN_POINT ( 'NONE',  ( 13.00000000000000178, 0.7793280607715257213, 4.825575716215943167 ) ) ;
#14173 = SURFACE_SIDE_STYLE ('',( #8060 ) ) ;
#14174 = CARTESIAN_POINT ( 'NONE',  ( 2.789999999999999147, 24.44424927289185945, -0.2301004812058395077 ) ) ;
#14175 = ORIENTED_EDGE ( 'NONE', *, *, #12709, .F. ) ;
#14176 = EDGE_LOOP ( 'NONE', ( #14074, #8107, #10526, #1973, #14671 ) ) ;
#14177 = CARTESIAN_POINT ( 'NONE',  ( -2.850000000000058265, -4.936344801571268093, -6.000000000000005329 ) ) ;
#14178 = ADVANCED_FACE ( 'NONE', ( #1936 ), #18449, .F. ) ;
#14179 = AXIS2_PLACEMENT_3D ( 'NONE', #17712, #2587, #5591 ) ;
#14180 = B_SPLINE_CURVE_WITH_KNOTS ( 'NONE', 3,
 ( #14372, #4766, #3559, #6545, #8265, #14272 ),
 .UNSPECIFIED., .F., .F.,
 ( 4, 2, 4 ),
 ( 4.462636808903086370E-07, 0.001879885123572231417, 0.003759323983463572477 ),
 .UNSPECIFIED. ) ;
#14181 = CARTESIAN_POINT ( 'NONE',  ( 2.789999999999999147, 2.680914349914567470E-13, -25.59481291497571220 ) ) ;
#14182 = CARTESIAN_POINT ( 'NONE',  ( -4.888101187500000222, 0.7741991708318887166, -6.968749997951614539 ) ) ;
#14183 = VERTEX_POINT ( 'NONE', #4742 ) ;
#14184 = CARTESIAN_POINT ( 'NONE',  ( 14.34374999795161365, 4.780397808154273065, -1.280903732194386802 ) ) ;
#14185 = DIRECTION ( 'NONE',  ( 0.000000000000000000, 0.000000000000000000, -1.000000000000000000 ) ) ;
#14186 = CIRCLE ( 'NONE', #7137, 22.00000000000000355 ) ;
#14187 = VERTEX_POINT ( 'NONE', #447 ) ;
#14188 = DIRECTION ( 'NONE',  ( 1.000000000000000000, -0.000000000000000000, -0.000000000000000000 ) ) ;
#14189 = CARTESIAN_POINT ( 'NONE',  ( 5.000000000000000000, -2.000000000000001776, 41.99999999999999289 ) ) ;
#14190 = AXIS2_PLACEMENT_3D ( 'NONE', #12994, #10187, #9998 ) ;
#14191 = FACE_OUTER_BOUND ( 'NONE', #17155, .T. ) ;
#14192 = DIRECTION ( 'NONE',  ( 1.000000000000000000, 0.000000000000000000, 0.000000000000000000 ) ) ;
#14193 = EDGE_CURVE ( 'NONE', #9700, #7035, #14481, .T. ) ;
#14194 = CARTESIAN_POINT ( 'NONE',  ( -3.383411828340740850E-14, -4.888101187500000222, -11.46874999795161543 ) ) ;
#14195 = EDGE_LOOP ( 'NONE', ( #13731, #15066, #9591, #1326 ) ) ;
#14196 = DIRECTION ( 'NONE',  ( 0.000000000000000000, 0.000000000000000000, 1.000000000000000000 ) ) ;
#14197 = CARTESIAN_POINT ( 'NONE',  ( 0.07181524296601451973, 16.91181672897733534, 18.89296398180198011 ) ) ;
#14198 = FILL_AREA_STYLE ('',( #6674 ) ) ;
#14199 = ORIENTED_EDGE ( 'NONE', *, *, #5280, .T. ) ;
#14200 = PLANE ( 'NONE',  #4716 ) ;
#14201 = EDGE_CURVE ( 'NONE', #13977, #759, #17870, .T. ) ;
#14202 = AXIS2_PLACEMENT_3D ( 'NONE', #11272, #11070, #11173 ) ;
#14203 = CARTESIAN_POINT ( 'NONE',  ( 2.790000000000077307, -5.456611084821691549, -23.69897269326682832 ) ) ;
#14204 = PRODUCT_DEFINITION_CONTEXT ( 'detailed design', #4709, 'design' ) ;
#14205 = FACE_OUTER_BOUND ( 'NONE', #4882, .T. ) ;
#14206 = CARTESIAN_POINT ( 'NONE',  ( 22.00000000000000355, 2.694222958124177204E-15, -35.00000000000000000 ) ) ;
#14207 = CARTESIAN_POINT ( 'NONE',  ( 6.468749997951615427, -4.233219804643904460, 2.444050593749960587 ) ) ;
#14208 = ORIENTED_EDGE ( 'NONE', *, *, #1205, .T. ) ;
#14209 = ADVANCED_FACE ( 'NONE', ( #10852 ), #12949, .F. ) ;
#14210 = FACE_OUTER_BOUND ( 'NONE', #11857, .T. ) ;
#14211 = CARTESIAN_POINT ( 'NONE',  ( 2.789999999999999147, -7.909232158574647009, -24.34211360614308006 ) ) ;
#14212 = ORIENTED_EDGE ( 'NONE', *, *, #13441, .T. ) ;
#14213 = AXIS2_PLACEMENT_3D ( 'NONE', #13116, #14626, #823 ) ;
#14214 = CARTESIAN_POINT ( 'NONE',  ( 2.000000000000001776, 0.000000000000000000, 0.000000000000000000 ) ) ;
#14215 = CARTESIAN_POINT ( 'NONE',  ( 4.999999999999963585, 7.196152422706642682, 37.99999999999999289 ) ) ;
#14216 = VERTEX_POINT ( 'NONE', #17643 ) ;
#14217 = ADVANCED_FACE ( 'NONE', ( #6921 ), #2234, .F. ) ;
#14218 = CIRCLE ( 'NONE', #9109, 9.000000000000001776 ) ;
#14219 = CARTESIAN_POINT ( 'NONE',  ( 2.718131885465892683, -18.89333555428565603, 16.91241718341992240 ) ) ;
#14220 = CARTESIAN_POINT ( 'NONE',  ( 0.000000000000000000, 0.000000000000000000, -6.502399999999998847 ) ) ;
#14221 = VERTEX_POINT ( 'NONE', #16153 ) ;
#14222 = DIRECTION ( 'NONE',  ( -1.000000000000000000, 0.000000000000000000, 0.000000000000000000 ) ) ;
#14223 = CARTESIAN_POINT ( 'NONE',  ( -15.00000000000000355, 3.434748899119118626, 2.750000000000001332 ) ) ;
#14224 = EDGE_CURVE ( 'NONE', #4306, #12283, #5552, .T. ) ;
#14225 = CARTESIAN_POINT ( 'NONE',  ( 2.246813503491833508, 4.409619785863906571, -12.96874999795161543 ) ) ;
#14226 = ORIENTED_EDGE ( 'NONE', *, *, #1214, .T. ) ;
#14227 = PLANE ( 'NONE',  #1921 ) ;
#14228 = ORIENTED_EDGE ( 'NONE', *, *, #7818, .F. ) ;
#14229 = CARTESIAN_POINT ( 'NONE',  ( 2.604434514863827488, -23.63475234378990208, 10.67816411292155543 ) ) ;
#14230 = ORIENTED_EDGE ( 'NONE', *, *, #631, .F. ) ;
#14231 = FACE_OUTER_BOUND ( 'NONE', #5186, .T. ) ;
#14232 = CARTESIAN_POINT ( 'NONE',  ( -3.846120219227966430, -3.114526743279228072, -11.34374999795161543 ) ) ;
#14233 = DIRECTION ( 'NONE',  ( 0.000000000000000000, 0.000000000000000000, 1.000000000000000000 ) ) ;
#14234 = AXIS2_PLACEMENT_3D ( 'NONE', #17880, #11875, #17987 ) ;
#14235 = EDGE_CURVE ( 'NONE', #6609, #5566, #13043, .T. ) ;
#14236 = CARTESIAN_POINT ( 'NONE',  ( 2.789999999999999147, 1.991882183130294637, 24.04302995059966364 ) ) ;
#14237 = AXIS2_PLACEMENT_3D ( 'NONE', #19139, #2333, #935 ) ;
#14238 = EDGE_LOOP ( 'NONE', ( #18886, #18081 ) ) ;
#14239 = CARTESIAN_POINT ( 'NONE',  ( -0.000000000000000000, 0.000000000000000000, 0.000000000000000000 ) ) ;
#14240 = LINE ( 'NONE', #739, #19671 ) ;
#14241 = ORIENTED_EDGE ( 'NONE', *, *, #18752, .F. ) ;
#14242 = ADVANCED_FACE ( 'NONE', ( #646 ), #4033, .T. ) ;
#14243 = B_SPLINE_CURVE_WITH_KNOTS ( 'NONE', 3,
 ( #12305, #18402, #3189, #15403 ),
 .UNSPECIFIED., .F., .F.,
 ( 4, 4 ),
 ( 0.005258214619651960589, 0.005948481662034167325 ),
 .UNSPECIFIED. ) ;
#14244 = CARTESIAN_POINT ( 'NONE',  ( -9.580134541264520465, -14.56230589874905235, 32.00000000000000000 ) ) ;
#14245 = DIRECTION ( 'NONE',  ( -1.000000000000000000, -6.419766481290786633E-33, 0.000000000000000000 ) ) ;
#14246 = CARTESIAN_POINT ( 'NONE',  ( 1.773574444220693103, -4.620319390059842490, -6.968749997951614539 ) ) ;
#14247 = VERTEX_POINT ( 'NONE', #8448 ) ;
#14248 = AXIS2_PLACEMENT_3D ( 'NONE', #17363, #11462, #2348 ) ;
#14249 = CARTESIAN_POINT ( 'NONE',  ( -1.886022603841296830, 0.000000000000000000, 0.000000000000000000 ) ) ;
#14250 = PLANE ( 'NONE',  #2413 ) ;
#14251 = DIRECTION ( 'NONE',  ( -0.000000000000000000, 0.000000000000000000, 1.000000000000000000 ) ) ;
#14252 = AXIS2_PLACEMENT_3D ( 'NONE', #9072, #10673, #19563 ) ;
#14253 = ORIENTED_EDGE ( 'NONE', *, *, #8136, .F. ) ;
#14254 = CARTESIAN_POINT ( 'NONE',  ( 2.789999999999999147, -20.70663861606282197, 15.04425356660753188 ) ) ;
#14255 = EDGE_LOOP ( 'NONE', ( #2453, #19042 ) ) ;
#14256 = APPLICATION_PROTOCOL_DEFINITION ( 'draft international standard', 'automotive_design', 1998, #12132 ) ;
#14257 = DIRECTION ( 'NONE',  ( -1.000000000000000000, -6.419766481290786633E-33, 0.000000000000000000 ) ) ;
#14258 = LINE ( 'NONE', #9769, #19463 ) ;
#14259 = ORIENTED_EDGE ( 'NONE', *, *, #503, .T. ) ;
#14260 = EDGE_LOOP ( 'NONE', ( #9753, #11806, #2212, #9101 ) ) ;
#14261 = DIRECTION ( 'NONE',  ( 1.000000000000000000, 0.000000000000000000, 0.000000000000000000 ) ) ;
#14262 = CARTESIAN_POINT ( 'NONE',  ( 10.46874999795161720, -1.016293382781444654, 4.781284448697187273 ) ) ;
#14263 = ORIENTED_EDGE ( 'NONE', *, *, #3917, .T. ) ;
#14264 = CIRCLE ( 'NONE', #9149, 24.12539914357697768 ) ;
#14265 = AXIS2_PLACEMENT_3D ( 'NONE', #2512, #11723, #5706 ) ;
#14266 = CARTESIAN_POINT ( 'NONE',  ( -4.942249507334554259, 0.2590123213421660631, -10.34374999795161543 ) ) ;
#14267 = EDGE_CURVE ( 'NONE', #1526, #3097, #13544, .T. ) ;
#14268 = VERTEX_POINT ( 'NONE', #19043 ) ;
#14269 = CARTESIAN_POINT ( 'NONE',  ( -18.96448111170889206, 1.130229351527647808, 32.00000000000000000 ) ) ;
#14270 = EDGE_CURVE ( 'NONE', #13330, #5965, #836, .T. ) ;
#14271 = CARTESIAN_POINT ( 'NONE',  ( 10.00000000000000533, -5.421022142882388373, 1.761396867937162769 ) ) ;
#14272 = CARTESIAN_POINT ( 'NONE',  ( 2.765633920072235963, -16.37294372382871188, 18.55949924794887096 ) ) ;
#14273 = AXIS2_PLACEMENT_3D ( 'NONE', #6868, #3985, #17400 ) ;
#14274 = ORIENTED_EDGE ( 'NONE', *, *, #5204, .T. ) ;
#14275 = CARTESIAN_POINT ( 'NONE',  ( -11.00000000000000355, -4.215373648918918192, 3.375000000000000888 ) ) ;
#14276 = FACE_OUTER_BOUND ( 'NONE', #18176, .T. ) ;
#14277 = AXIS2_PLACEMENT_3D ( 'NONE', #19489, #5778, #11897 ) ;
#14278 = VERTEX_POINT ( 'NONE', #12749 ) ;
#14279 = ORIENTED_EDGE ( 'NONE', *, *, #17097, .F. ) ;
#14280 = CARTESIAN_POINT ( 'NONE',  ( 11.32184790671639263, 13.12143529358541016, -35.00000000000000000 ) ) ;
#14281 = EDGE_CURVE ( 'NONE', #1617, #11735, #3365, .T. ) ;
#14282 = DIRECTION ( 'NONE',  ( 1.000000000000000000, -0.000000000000000000, -0.000000000000000000 ) ) ;
#14283 = DIRECTION ( 'NONE',  ( -1.000000000000000000, 0.000000000000000000, 0.000000000000000000 ) ) ;
#14284 = EDGE_LOOP ( 'NONE', ( #5466, #14083, #9112, #11211 ) ) ;
#14285 = DIRECTION ( 'NONE',  ( 0.000000000000000000, 0.000000000000000000, -1.000000000000000000 ) ) ;
#14286 = DIRECTION ( 'NONE',  ( -0.000000000000000000, -0.000000000000000000, 1.000000000000000000 ) ) ;
#14287 = AXIS2_PLACEMENT_3D ( 'NONE', #14842, #5156, #11073 ) ;
#14288 = EDGE_LOOP ( 'NONE', ( #11555, #7957, #14987, #4755 ) ) ;
#14289 = FACE_OUTER_BOUND ( 'NONE', #11863, .T. ) ;
#14290 = CIRCLE ( 'NONE', #17478, 1.000000000000002665 ) ;
#14291 = CARTESIAN_POINT ( 'NONE',  ( 11.00000000000000711, 5.700000000000001066, -3.490243377569957047E-16 ) ) ;
#14292 = ADVANCED_FACE ( 'NONE', ( #17451 ), #1411, .T. ) ;
#14293 = CARTESIAN_POINT ( 'NONE',  ( -15.00000000000000355, 4.874999999999998224, 3.903123748998999165 ) ) ;
#14294 = CARTESIAN_POINT ( 'NONE',  ( 0.02436607992776281678, 2.336989772644269436, 24.63872515616083447 ) ) ;
#14295 = CARTESIAN_POINT ( 'NONE',  ( -3.945386292505473391E-14, -5.700000000000001066, -11.00000000000000711 ) ) ;
#14296 = CARTESIAN_POINT ( 'NONE',  ( 8.000000000000000000, 1.999999999999997335, 37.99999999999999289 ) ) ;
#14297 = DIRECTION ( 'NONE',  ( -0.000000000000000000, -0.000000000000000000, 1.000000000000000000 ) ) ;
#14298 = CARTESIAN_POINT ( 'NONE',  ( -0.3020334839682480288, 5.763142191869157216, -8.812499995903225525 ) ) ;
#14299 = ORIENTED_EDGE ( 'NONE', *, *, #5204, .F. ) ;
#14300 = CARTESIAN_POINT ( 'NONE',  ( -1.255998204157475318, -17.85806462366060288, -32.00000000000000000 ) ) ;
#14301 = AXIS2_PLACEMENT_3D ( 'NONE', #7990, #3497, #6575 ) ;
#14302 = LINE ( 'NONE', #9813, #4255 ) ;
#14303 = CARTESIAN_POINT ( 'NONE',  ( 2.789999999999999147, 12.59161484032942901, -21.30679549418617924 ) ) ;
#14304 = VECTOR ( 'NONE', #13271, 1000.000000000000000 ) ;
#14305 = CARTESIAN_POINT ( 'NONE',  ( 2.789999999999999147, -20.70663861606260170, -15.04425356660783031 ) ) ;
#14306 = DIRECTION ( 'NONE',  ( -0.000000000000000000, -0.000000000000000000, 1.000000000000000000 ) ) ;
#14307 = ORIENTED_EDGE ( 'NONE', *, *, #2761, .T. ) ;
#14308 = CARTESIAN_POINT ( 'NONE',  ( 8.000000000000000000, 0.000000000000000000, 0.000000000000000000 ) ) ;
#14309 = CARTESIAN_POINT ( 'NONE',  ( 1.394999999999999574, -12.96210679857767900, -24.89775460606846380 ) ) ;
#14310 = ORIENTED_EDGE ( 'NONE', *, *, #13545, .F. ) ;
#14311 = CARTESIAN_POINT ( 'NONE',  ( 10.34374999795161543, -4.409619785863921670, 2.246813503491803310 ) ) ;
#14312 = EDGE_CURVE ( 'NONE', #5054, #4468, #9910, .T. ) ;
#14313 = EDGE_CURVE ( 'NONE', #6761, #17056, #10142, .T. ) ;
#14314 = DIRECTION ( 'NONE',  ( 1.000000000000000000, 0.000000000000000000, 0.000000000000000000 ) ) ;
#14315 = ORIENTED_EDGE ( 'NONE', *, *, #7221, .F. ) ;
#14316 = DIRECTION ( 'NONE',  ( 1.000000000000000000, -0.000000000000000000, -0.000000000000000000 ) ) ;
#14317 = ADVANCED_FACE ( 'NONE', ( #5130 ), #16240, .F. ) ;
#14318 = AXIS2_PLACEMENT_3D ( 'NONE', #11080, #1578, #7667 ) ;
#14319 = AXIS2_PLACEMENT_3D ( 'NONE', #16324, #14436, #6907 ) ;
#14320 = CARTESIAN_POINT ( 'NONE',  ( 5.510910596163084625E-16, 18.00000000000000355, -35.00000000000000000 ) ) ;
#14321 = CARTESIAN_POINT ( 'NONE',  ( 10.81249999590322375, 5.142044285764750811, -2.620002426024544473 ) ) ;
#14322 = ORIENTED_EDGE ( 'NONE', *, *, #3788, .F. ) ;
#14323 = CARTESIAN_POINT ( 'NONE',  ( 2.499999999999999112, 6.200000000000021494, 0.000000000000000000 ) ) ;
#14324 = CARTESIAN_POINT ( 'NONE',  ( 1.394999999999999574, -4.633866840649122132, 27.68468304288257542 ) ) ;
#14325 = CARTESIAN_POINT ( 'NONE',  ( 3.954556930911861112, 2.873153789725825913, -14.46874999795161720 ) ) ;
#14326 = ORIENTED_EDGE ( 'NONE', *, *, #12099, .T. ) ;
#14327 = CYLINDRICAL_SURFACE ( 'NONE', #2885, 1.000000000000000000 ) ;
#14328 = ORIENTED_EDGE ( 'NONE', *, *, #15473, .F. ) ;
#14329 = CARTESIAN_POINT ( 'NONE',  ( -41.99999999999999289, -5.000000000000001776, -2.000000000000000000 ) ) ;
#14330 = VERTEX_POINT ( 'NONE', #3637 ) ;
#14331 = CARTESIAN_POINT ( 'NONE',  ( -2.000000000000001776, -3.218695387886217674, 2.999999999999999112 ) ) ;
#14332 = LINE ( 'NONE', #6707, #11407 ) ;
#14333 = DIRECTION ( 'NONE',  ( 0.000000000000000000, 0.000000000000000000, 1.000000000000000000 ) ) ;
#14334 = AXIS2_PLACEMENT_3D ( 'NONE', #10883, #9285, #7773 ) ;
#14335 = CARTESIAN_POINT ( 'NONE',  ( 4.233219804643871598, -2.444050593750019651, -11.84374999795161365 ) ) ;
#14336 = ORIENTED_EDGE ( 'NONE', *, *, #11692, .F. ) ;
#14337 = CARTESIAN_POINT ( 'NONE',  ( 10.58013454126452046, -14.56230589874905412, 35.00000000000000000 ) ) ;
#14338 = CARTESIAN_POINT ( 'NONE',  ( 2.765633920072239516, 21.30679549418631780, 12.59161484032919986 ) ) ;
#14339 = EDGE_LOOP ( 'NONE', ( #2286, #454 ) ) ;
#14340 = FACE_BOUND ( 'NONE', #6219, .T. ) ;
#14341 = EDGE_CURVE ( 'NONE', #2962, #16730, #11322, .T. ) ;
#14342 = DIRECTION ( 'NONE',  ( -1.000000000000000000, -0.000000000000000000, -0.000000000000000000 ) ) ;
#14343 = DIRECTION ( 'NONE',  ( -0.000000000000000000, -0.000000000000000000, 1.000000000000000000 ) ) ;
#14344 = EDGE_CURVE ( 'NONE', #12535, #3914, #9861, .T. ) ;
#14345 = AXIS2_PLACEMENT_3D ( 'NONE', #511, #402, #6481 ) ;
#14346 = ORIENTED_EDGE ( 'NONE', *, *, #1010, .T. ) ;
#14347 = CARTESIAN_POINT ( 'NONE',  ( 0.5279273620711150139, 23.73240184472514613, -12.96450951081191150 ) ) ;
#14348 = CARTESIAN_POINT ( 'NONE',  ( 3.499494075959792116, -3.499494075959840966, -8.968749997951613651 ) ) ;
#14349 = CARTESIAN_POINT ( 'NONE',  ( 1.749999999999998002, -24.89775460606821866, -12.96210679857815684 ) ) ;
#14350 = ORIENTED_EDGE ( 'NONE', *, *, #17815, .F. ) ;
#14351 = CARTESIAN_POINT ( 'NONE',  ( -15.19790265903627180, 9.644882309621941374, -32.00000000000000000 ) ) ;
#14352 = ORIENTED_EDGE ( 'NONE', *, *, #16681, .T. ) ;
#14353 = ITEM_DEFINED_TRANSFORMATION ( 'NONE', 'NONE', #10840,  #16724 ) ;
#14354 = LINE ( 'NONE', #11545, #6458 ) ;
#14355 = AXIS2_PLACEMENT_3D ( 'NONE', #16365, #9062, #15161 ) ;
#14356 = DIRECTION ( 'NONE',  ( 0.000000000000000000, 0.000000000000000000, -1.000000000000000000 ) ) ;
#14357 = ADVANCED_FACE ( 'NONE', ( #14933 ), #16736, .T. ) ;
#14358 = EDGE_LOOP ( 'NONE', ( #352, #3542, #6702, #1035 ) ) ;
#14359 =( BOUNDED_CURVE ( )  B_SPLINE_CURVE ( 2, ( #496, #7983, #6569, #12697, #18791, #1081, #7156, #9906, #6965, #887, #17689, #4179, #12995, #5763, #13190 ),
 .UNSPECIFIED., .F., .F. ) 
 B_SPLINE_CURVE_WITH_KNOTS ( ( 3, 2, 2, 2, 2, 2, 2, 3 ),
 ( 0.000000000000000000, 0.05000000000000000278, 0.1000000000000000056, 0.1499999999999999944, 0.2000000000000000111, 0.2500000000000000000, 0.2999999999999999889, 0.3078686208676164604 ),
 .UNSPECIFIED. ) 
 CURVE ( )  GEOMETRIC_REPRESENTATION_ITEM ( )  RATIONAL_B_SPLINE_CURVE ( ( 1.000000000000000000, 0.9876883405951377704, 1.000000000000000000, 0.9876883405951377704, 1.000000000000000000, 0.9876883405951377704, 1.000000000000000000, 0.9876883405951377704, 1.000000000000000000, 0.9876883405951377704, 1.000000000000000000, 0.9876883405951377704, 1.000000000000000000, 0.9980624843978382899, 0.9967347918236166837 ) ) 
 REPRESENTATION_ITEM ( '' )  );
#14360 = ORIENTED_EDGE ( 'NONE', *, *, #5537, .F. ) ;
#14361 = DIRECTION ( 'NONE',  ( -1.000000000000000000, -0.000000000000000000, -0.000000000000000000 ) ) ;
#14362 = DIRECTION ( 'NONE',  ( 1.000000000000000000, 0.000000000000000000, 0.000000000000000000 ) ) ;
#14363 = CARTESIAN_POINT ( 'NONE',  ( 6.968749997951614539, 3.846120219227923798, 3.114526743279282694 ) ) ;
#14364 = EDGE_LOOP ( 'NONE', ( #9510, #13038, #15164, #17211 ) ) ;
#14365 = ADVANCED_FACE ( 'NONE', ( #12133 ), #13186, .T. ) ;
#14366 = EDGE_CURVE ( 'NONE', #2117, #19129, #18136, .T. ) ;
#14367 =( LENGTH_UNIT ( ) NAMED_UNIT ( * ) SI_UNIT ( .MILLI., .METRE. ) );
#14368 = EDGE_LOOP ( 'NONE', ( #10107, #17118 ) ) ;
#14369 = EDGE_CURVE ( 'NONE', #3518, #17740, #5640, .T. ) ;
#14370 = DIRECTION ( 'NONE',  ( 1.000000000000000000, 0.000000000000000000, -0.000000000000000000 ) ) ;
#14371 = CARTESIAN_POINT ( 'NONE',  ( 11.00000000000000711, -5.700000000000001066, -3.945386292505473391E-14 ) ) ;
#14372 = CARTESIAN_POINT ( 'NONE',  ( 1.749999999999998002, -19.67366047555544739, 20.02152543075338897 ) ) ;
#14373 = VERTEX_POINT ( 'NONE', #19629 ) ;
#14374 = DIRECTION ( 'NONE',  ( 0.000000000000000000, 0.000000000000000000, 1.000000000000000000 ) ) ;
#14375 =( NAMED_UNIT ( * ) SI_UNIT ( $, .STERADIAN. ) SOLID_ANGLE_UNIT ( ) );
#14376 = DIRECTION ( 'NONE',  ( -1.000000000000000000, -0.000000000000000000, -0.000000000000000000 ) ) ;
#14377 = EDGE_CURVE ( 'NONE', #3153, #11007, #10601, .T. ) ;
#14378 = ORIENTED_EDGE ( 'NONE', *, *, #5496, .F. ) ;
#14379 = VERTEX_POINT ( 'NONE', #4129 ) ;
#14380 = CARTESIAN_POINT ( 'NONE',  ( -5.668774803599165857, -0.5958122406255588199, -9.000000000000005329 ) ) ;
#14381 = AXIS2_PLACEMENT_3D ( 'NONE', #13637, #19733, #10738 ) ;
#14382 = B_SPLINE_CURVE_WITH_KNOTS ( 'NONE', 3,
 ( #12055, #1446, #18446, #9152 ),
 .UNSPECIFIED., .F., .F.,
 ( 4, 4 ),
 ( 0.000000000000000000, 0.001126652051248517921 ),
 .UNSPECIFIED. ) ;
#14383 = AXIS2_PLACEMENT_3D ( 'NONE', #19431, #7406, #7209 ) ;
#14384 = FACE_OUTER_BOUND ( 'NONE', #10022, .T. ) ;
#14385 = EDGE_CURVE ( 'NONE', #3518, #7686, #10531, .T. ) ;
#14386 = DIRECTION ( 'NONE',  ( 1.000000000000000000, 0.000000000000000000, 0.000000000000000000 ) ) ;
#14387 = EDGE_CURVE ( 'NONE', #16939, #18923, #19418, .T. ) ;
#14388 = ORIENTED_EDGE ( 'NONE', *, *, #18360, .F. ) ;
#14389 = LINE ( 'NONE', #18682, #13800 ) ;
#14390 = CARTESIAN_POINT ( 'NONE',  ( 11.34374999795161543, 1.773574444220789914, -4.620319390059805187 ) ) ;
#14391 = ORIENTED_EDGE ( 'NONE', *, *, #861, .F. ) ;
#14392 = DIRECTION ( 'NONE',  ( 0.000000000000000000, 0.000000000000000000, 1.000000000000000000 ) ) ;
#14393 = CYLINDRICAL_SURFACE ( 'NONE', #13450, 22.00000000000000355 ) ;
#14394 = VECTOR ( 'NONE', #14407, 1000.000000000000000 ) ;
#14395 = EDGE_CURVE ( 'NONE', #6321, #8931, #7676, .T. ) ;
#14396 = AXIS2_PLACEMENT_3D ( 'NONE', #10902, #4797, #3398 ) ;
#14397 = DIRECTION ( 'NONE',  ( -0.000000000000000000, -0.000000000000000000, 1.000000000000000000 ) ) ;
#14398 = DIRECTION ( 'NONE',  ( 1.000000000000000000, 0.000000000000000000, 0.000000000000000000 ) ) ;
#14399 = DIRECTION ( 'NONE',  ( 0.000000000000000000, -1.000000000000000000, 0.000000000000000000 ) ) ;
#14400 = CARTESIAN_POINT ( 'NONE',  ( -30.00000000000000000, 1.224646799147352468E-16, 0.000000000000000000 ) ) ;
#14401 = CARTESIAN_POINT ( 'NONE',  ( 7.937500000000000000, -1.543790678740078581, -0.06656457167770415961 ) ) ;
#14402 = CARTESIAN_POINT ( 'NONE',  ( 1.493657965219523875, 5.574407415329157622, -9.812499995903225525 ) ) ;
#14403 = ORIENTED_EDGE ( 'NONE', *, *, #13442, .T. ) ;
#14404 = DIRECTION ( 'NONE',  ( 1.000000000000000000, 0.000000000000000000, 0.000000000000000000 ) ) ;
#14405 = CARTESIAN_POINT ( 'NONE',  ( 2.262072769566602304, 11.57956866523218586, 24.43806413951680767 ) ) ;
#14406 = UNCERTAINTY_MEASURE_WITH_UNIT (LENGTH_MEASURE( 1.000000000000000082E-05 ), #17225, 'distance_accuracy_value', 'NONE');
#14407 = DIRECTION ( 'NONE',  ( -1.000000000000000000, 0.000000000000000000, -0.000000000000000000 ) ) ;
#14408 = CARTESIAN_POINT ( 'NONE',  ( 8.968749997951611874, -4.780397808154247308, -1.280903732194487166 ) ) ;
#14409 = EDGE_LOOP ( 'NONE', ( #18374, #1267, #4269, #8601 ) ) ;
#14410 = CARTESIAN_POINT ( 'NONE',  ( -16.28688694438836038, -7.664027248171298545, -32.00000000000000000 ) ) ;
#14411 = AXIS2_PLACEMENT_3D ( 'NONE', #7428, #17858, #41 ) ;
#14412 = CARTESIAN_POINT ( 'NONE',  ( -4.409619785863906571, 2.246813503491833508, -8.343749997951611874 ) ) ;
#14413 = ADVANCED_FACE ( 'NONE', ( #7882 ), #501, .T. ) ;
#14414 = EDGE_LOOP ( 'NONE', ( #13443, #1918 ) ) ;
#14415 = CYLINDRICAL_SURFACE ( 'NONE', #374, 13.19999999999999929 ) ;
#14416 = CARTESIAN_POINT ( 'NONE',  ( 2.789999999999999147, 12.52067188844351442, 20.62201879784917935 ) ) ;
#14417 = ORIENTED_EDGE ( 'NONE', *, *, #7227, .F. ) ;
#14418 = CARTESIAN_POINT ( 'NONE',  ( -8.671566133830875600, 15.77352024078954429, -32.00000000000000000 ) ) ;
#14419 = CARTESIAN_POINT ( 'NONE',  ( 1.999999999999998224, 0.000000000000000000, 0.000000000000000000 ) ) ;
#14420 = CARTESIAN_POINT ( 'NONE',  ( 0.000000000000000000, 15.74360496233383522, 18.28042085475283329 ) ) ;
#14421 = CARTESIAN_POINT ( 'NONE',  ( 2.789679245949058917, 20.70663861606308487, -12.51925356660738053 ) ) ;
#14422 = ORIENTED_EDGE ( 'NONE', *, *, #18069, .T. ) ;
#14423 = AXIS2_PLACEMENT_3D ( 'NONE', #11850, #17960, #6863 ) ;
#14424 = LINE ( 'NONE', #5311, #3389 ) ;
#14425 = DIRECTION ( 'NONE',  ( -1.000000000000000000, -0.000000000000000000, -0.000000000000000000 ) ) ;
#14426 = CONICAL_SURFACE ( 'NONE', #10909, 4.000000000000000000, 0.2132412839022289897 ) ;
#14427 = ORIENTED_EDGE ( 'NONE', *, *, #11774, .T. ) ;
#14428 = ADVANCED_FACE ( 'NONE', ( #15899 ), #13708, .T. ) ;
#14429 = CARTESIAN_POINT ( 'NONE',  ( -2.000000000000000000, -2.000000000000002665, 37.99999999999999289 ) ) ;
#14430 = ORIENTED_EDGE ( 'NONE', *, *, #11581, .T. ) ;
#14431 = CARTESIAN_POINT ( 'NONE',  ( 1.039999999999997593, 0.000000000000000000, 0.000000000000000000 ) ) ;
#14432 = ORIENTED_EDGE ( 'NONE', *, *, #17370, .T. ) ;
#14433 = FACE_OUTER_BOUND ( 'NONE', #5027, .T. ) ;
#14434 = CARTESIAN_POINT ( 'NONE',  ( 0.9027913098498565603, 5.700000000000000178, -12.81249999590322552 ) ) ;
#14435 = CARTESIAN_POINT ( 'NONE',  ( 2.789999999999999147, 21.30679549418649543, -12.59161484032888723 ) ) ;
#14436 = DIRECTION ( 'NONE',  ( 0.000000000000000000, 0.000000000000000000, 1.000000000000000000 ) ) ;
#14437 = EDGE_CURVE ( 'NONE', #8766, #1773, #7966, .T. ) ;
#14438 = ORIENTED_EDGE ( 'NONE', *, *, #19437, .T. ) ;
#14439 = FACE_BOUND ( 'NONE', #12646, .T. ) ;
#14440 = CARTESIAN_POINT ( 'NONE',  ( -0.5958122406255597081, 5.668774803599165857, -15.31249999590322552 ) ) ;
#14441 = AXIS2_PLACEMENT_3D ( 'NONE', #2712, #10339, #17544 ) ;
#14442 = EDGE_LOOP ( 'NONE', ( #18855, #6730, #18361, #16537 ) ) ;
#14443 = AXIS2_PLACEMENT_3D ( 'NONE', #8694, #18007, #7170 ) ;
#14444 = AXIS2_PLACEMENT_3D ( 'NONE', #14540, #15836, #2412 ) ;
#14445 = CARTESIAN_POINT ( 'NONE',  ( 0.02436607992775891365, -24.63872515616080960, -2.336989772644527008 ) ) ;
#14446 = DIRECTION ( 'NONE',  ( 1.000000000000000000, 0.000000000000000000, 0.000000000000000000 ) ) ;
#14447 = CARTESIAN_POINT ( 'NONE',  ( -3.954556930911881096, -2.873153789725797935, -14.84374999795161543 ) ) ;
#14448 = ORIENTED_EDGE ( 'NONE', *, *, #2834, .T. ) ;
#14449 = DIRECTION ( 'NONE',  ( 1.000000000000000000, 0.000000000000000000, 0.000000000000000000 ) ) ;
#14450 = DIRECTION ( 'NONE',  ( 0.000000000000000000, 0.000000000000000000, -1.000000000000000000 ) ) ;
#14451 = CARTESIAN_POINT ( 'NONE',  ( -5.207209108562804722, 2.318398865532109276, -15.31249999590322552 ) ) ;
#14452 = VERTEX_POINT ( 'NONE', #6669 ) ;
#14453 = EDGE_CURVE ( 'NONE', #11375, #5856, #14090, .T. ) ;
#14454 = CARTESIAN_POINT ( 'NONE',  ( 0.006931069955678950678, -18.43696893154746164, -16.17493693894899209 ) ) ;
#14455 = AXIS2_PLACEMENT_3D ( 'NONE', #10186, #16287, #2564 ) ;
#14456 = ORIENTED_EDGE ( 'NONE', *, *, #12401, .F. ) ;
#14457 = VECTOR ( 'NONE', #86, 1000.000000000000114 ) ;
#14458 = CARTESIAN_POINT ( 'NONE',  ( 13.00000000000000000, -5.567819778318897406, -1.220402768007724292 ) ) ;
#14459 = SURFACE_STYLE_USAGE ( .BOTH. , #944 ) ;
#14460 = CIRCLE ( 'NONE', #10626, 5.400000000000000355 ) ;
#14461 = DIRECTION ( 'NONE',  ( 1.000000000000000000, 0.000000000000000000, 0.000000000000000000 ) ) ;
#14462 = ORIENTED_EDGE ( 'NONE', *, *, #19413, .F. ) ;
#14463 = ORIENTED_EDGE ( 'NONE', *, *, #17955, .F. ) ;
#14464 = CARTESIAN_POINT ( 'NONE',  ( 4.888101187500000222, -3.413342815706642518E-14, -6.843749997951615427 ) ) ;
#14465 = CARTESIAN_POINT ( 'NONE',  ( 11.31249999590322375, -5.421022142882388373, 1.761396867937162769 ) ) ;
#14466 = CARTESIAN_POINT ( 'NONE',  ( 12.73273607671833929, -3.906077990787160559, 2.967013497617006834 ) ) ;
#14467 = ORIENTED_EDGE ( 'NONE', *, *, #4667, .F. ) ;
#14468 = EDGE_CURVE ( 'NONE', #5313, #8529, #8161, .T. ) ;
#14469 = AXIS2_PLACEMENT_3D ( 'NONE', #12679, #10880, #4870 ) ;
#14470 = EDGE_CURVE ( 'NONE', #2028, #3546, #5179, .T. ) ;
#14471 = CARTESIAN_POINT ( 'NONE',  ( -3.000000000000001332, 10.00000000000000000, 0.000000000000000000 ) ) ;
#14472 = AXIS2_PLACEMENT_3D ( 'NONE', #6443, #3162, #17268 ) ;
#14473 = EDGE_LOOP ( 'NONE', ( #11905, #8873, #19100, #18670 ) ) ;
#14474 = MECHANICAL_DESIGN_GEOMETRIC_PRESENTATION_REPRESENTATION (  '', ( #18930 ), #6217 ) ;
#14475 = AXIS2_PLACEMENT_3D ( 'NONE', #11312, #17412, #6976 ) ;
#14476 = EDGE_CURVE ( 'NONE', #8156, #10630, #14359, .T. ) ;
#14477 = CIRCLE ( 'NONE', #4880, 8.239200000000002078 ) ;
#14478 = CARTESIAN_POINT ( 'NONE',  ( -10.58013454126452224, -14.56230589874905235, -32.00000000000000000 ) ) ;
#14479 = AXIS2_PLACEMENT_3D ( 'NONE', #18455, #9361, #7843 ) ;
#14480 = CARTESIAN_POINT ( 'NONE',  ( 11.50000000000000355, -5.699999999999994849, -0.9027913098498963063 ) ) ;
#14481 =( BOUNDED_CURVE ( )  B_SPLINE_CURVE ( 2, ( #6136, #6523, #16861, #3345, #12653, #13853, #9456, #15553, #18744, #5038, #11150, #17247, #15360, #8140, #146 ),
 .UNSPECIFIED., .F., .F. ) 
 B_SPLINE_CURVE_WITH_KNOTS ( ( 3, 2, 2, 2, 2, 2, 2, 3 ),
 ( 0.000000000000000000, 0.04999999999999999584, 0.09999999999999999167, 0.1499999999999999944, 0.1999999999999999833, 0.2500000000000000000, 0.2999999999999999889, 0.3499999999999999778 ),
 .UNSPECIFIED. ) 
 CURVE ( )  GEOMETRIC_REPRESENTATION_ITEM ( )  RATIONAL_B_SPLINE_CURVE ( ( 1.000000000000000000, 0.9876883405951377704, 1.000000000000000000, 0.9876883405951377704, 1.000000000000000000, 0.9876883405951377704, 1.000000000000000000, 0.9876883405951377704, 1.000000000000000000, 0.9876883405951377704, 1.000000000000000000, 0.9876883405951377704, 1.000000000000000000, 0.9876883405951377704, 1.000000000000000000 ) ) 
 REPRESENTATION_ITEM ( '' )  );
#14482 = CARTESIAN_POINT ( 'NONE',  ( -1.988169868018530906, 4.465502636338051445, -13.84374999795161543 ) ) ;
#14483 = EDGE_CURVE ( 'NONE', #11614, #13582, #8113, .T. ) ;
#14484 = SURFACE_STYLE_FILL_AREA ( #12974 ) ;
#14486 = EDGE_CURVE ( 'NONE', #15, #18486, #16517, .T. ) ;
#14485 = ADVANCED_FACE ( 'NONE', ( #13282 ), #3964, .T. ) ;
#14487 = CARTESIAN_POINT ( 'NONE',  ( 4.781284448697194378, 1.016293382781411792, -12.46874999795161543 ) ) ;
#14488 = EDGE_LOOP ( 'NONE', ( #17582, #4775 ) ) ;
#14489 = ORIENTED_EDGE ( 'NONE', *, *, #12667, .T. ) ;
#14490 = CARTESIAN_POINT ( 'NONE',  ( -5.575441324182679459, 1.185096637661293251, -10.00000000000000533 ) ) ;
#14491 = CIRCLE ( 'NONE', #425, 22.00000000000000355 ) ;
#14492 = CARTESIAN_POINT ( 'NONE',  ( 13.00000000000000178, 3.830176896397430752, -3.037670790816736410 ) ) ;
#14493 = VECTOR ( 'NONE', #13524, 1000.000000000000114 ) ;
#14494 = DIRECTION ( 'NONE',  ( 1.000000000000000000, 0.000000000000000000, 0.000000000000000000 ) ) ;
#14495 = EDGE_LOOP ( 'NONE', ( #14813, #11537, #18045, #1283 ) ) ;
#14496 = CARTESIAN_POINT ( 'NONE',  ( 14.46874999795161720, 4.861323657744413218, -0.5109457054261112852 ) ) ;
#14497 = CIRCLE ( 'NONE', #2979, 22.00000000000000355 ) ;
#14498 = DIRECTION ( 'NONE',  ( 1.000000000000000000, 0.000000000000000000, 0.000000000000000000 ) ) ;
#14499 = ORIENTED_EDGE ( 'NONE', *, *, #9837, .T. ) ;
#14500 = CARTESIAN_POINT ( 'NONE',  ( 0.000000000000000000, 0.000000000000000000, -22.00000000000000000 ) ) ;
#14501 = DIRECTION ( 'NONE',  ( 0.000000000000000000, 0.000000000000000000, -1.000000000000000000 ) ) ;
#14502 = PRESENTATION_LAYER_ASSIGNMENT (  '', '', ( #3306 ) ) ;
#14503 = CARTESIAN_POINT ( 'NONE',  ( -17.11901729331276911, 5.562305898749051458, 35.00000000000000000 ) ) ;
#14504 = CYLINDRICAL_SURFACE ( 'NONE', #14190, 13.19999999999999929 ) ;
#14505 = DIRECTION ( 'NONE',  ( -0.000000000000000000, -0.000000000000000000, 1.000000000000000000 ) ) ;
#14506 = PRODUCT_DEFINITION_SHAPE ( 'NONE', 'NONE',  #1614 ) ;
#14507 = CARTESIAN_POINT ( 'NONE',  ( -3.207603742328077057E-13, 82.80384757729329692, 37.99999999999999289 ) ) ;
#14508 = DIRECTION ( 'NONE',  ( 1.000000000000000000, 0.000000000000000000, 0.000000000000000000 ) ) ;
#14509 = AXIS2_PLACEMENT_3D ( 'NONE', #6393, #18620, #15625 ) ;
#14510 = FACE_OUTER_BOUND ( 'NONE', #15669, .T. ) ;
#14511 = EDGE_LOOP ( 'NONE', ( #5491, #5719, #19535, #16272 ) ) ;
#14512 = LINE ( 'NONE', #14697, #17185 ) ;
#14513 = CARTESIAN_POINT ( 'NONE',  ( -16.28688694438836038, -7.664027248171298545, -32.00000000000000000 ) ) ;
#14514 = CARTESIAN_POINT ( 'NONE',  ( 3.114526743279282694, 3.846120219227923798, -7.343749997951615427 ) ) ;
#14515 = CARTESIAN_POINT ( 'NONE',  ( 7.468749997951615427, -4.781284448697200595, 1.016293382781377819 ) ) ;
#14516 = CARTESIAN_POINT ( 'NONE',  ( 2.765633920072235963, 21.30679549418649543, -12.59161484032888723 ) ) ;
#14517 = CARTESIAN_POINT ( 'NONE',  ( 2.257825491203655055, -11.58891744060124473, 24.44564404695840665 ) ) ;
#14518 = EDGE_LOOP ( 'NONE', ( #12698, #4249 ) ) ;
#14519 = CARTESIAN_POINT ( 'NONE',  ( 14.81249999590322552, -4.080749450109621534, -4.080749450109677490 ) ) ;
#14520 = DIRECTION ( 'NONE',  ( -1.000000000000000000, -0.000000000000000000, -0.000000000000000000 ) ) ;
#14521 = ORIENTED_EDGE ( 'NONE', *, *, #2254, .F. ) ;
#14522 =( NAMED_UNIT ( * ) SI_UNIT ( $, .STERADIAN. ) SOLID_ANGLE_UNIT ( ) );
#14523 = AXIS2_PLACEMENT_3D ( 'NONE', #122, #15034, #10730 ) ;
#14524 = CARTESIAN_POINT ( 'NONE',  ( 2.257825459230520693, 4.993157874727810253, 26.58873630738054317 ) ) ;
#14525 = DIRECTION ( 'NONE',  ( 0.000000000000000000, 0.000000000000000000, -1.000000000000000000 ) ) ;
#14526 = ORIENTED_EDGE ( 'NONE', *, *, #8145, .T. ) ;
#14527 = VECTOR ( 'NONE', #1845, 1000.000000000000000 ) ;
#14528 = DIRECTION ( 'NONE',  ( 0.000000000000000000, 0.8660254037844432595, -0.4999999999999920619 ) ) ;
#14529 = SURFACE_STYLE_FILL_AREA ( #11808 ) ;
#14530 = DIRECTION ( 'NONE',  ( 1.000000000000000000, 0.000000000000000000, 0.000000000000000000 ) ) ;
#14531 = EDGE_CURVE ( 'NONE', #201, #18451, #12277, .T. ) ;
#14532 = EDGE_LOOP ( 'NONE', ( #19013, #8952, #11029, #13776, #14979, #10488, #15923, #12584 ) ) ;
#14533 = CARTESIAN_POINT ( 'NONE',  ( -5.700000000000001954, 6.980486755139915080E-16, 0.000000000000000000 ) ) ;
#14534 = EDGE_LOOP ( 'NONE', ( #7023, #7602, #6725, #11933 ) ) ;
#14535 = CARTESIAN_POINT ( 'NONE',  ( 7.812499995903224637, -5.387740456496247887, 2.068159791354145849 ) ) ;
#14536 = ORIENTED_EDGE ( 'NONE', *, *, #4960, .F. ) ;
#14537 = CARTESIAN_POINT ( 'NONE',  ( -7.810937420967753123E-14, 20.85287692521929159, 12.51293083811806461 ) ) ;
#14538 = AXIS2_PLACEMENT_3D ( 'NONE', #16221, #10120, #8706 ) ;
#14539 = CARTESIAN_POINT ( 'NONE',  ( 1.749999999999998002, 0.000000000000000000, 0.000000000000000000 ) ) ;
#14540 = CARTESIAN_POINT ( 'NONE',  ( -6.626241948324210540, -16.73597674598852336, 32.00000000000000000 ) ) ;
#14541 = CARTESIAN_POINT ( 'NONE',  ( 1.886022603841296608, 0.000000000000000000, 0.000000000000000000 ) ) ;
#14542 = EDGE_LOOP ( 'NONE', ( #9860, #4182, #16201, #17681 ) ) ;
#14543 = DIRECTION ( 'NONE',  ( -1.000000000000000000, -1.224646799147353207E-16, 0.000000000000000000 ) ) ;
#14544 = CARTESIAN_POINT ( 'NONE',  ( 16.28688694438835327, -7.664027248171309203, 35.00000000000000000 ) ) ;
#14545 = VECTOR ( 'NONE', #3705, 1000.000000000000000 ) ;
#14546 = ORIENTED_EDGE ( 'NONE', *, *, #9084, .T. ) ;
#14547 = ADVANCED_FACE ( 'NONE', ( #2566 ), #2470, .T. ) ;
#14548 = DIRECTION ( 'NONE',  ( 1.000000000000000000, 0.000000000000000000, 0.000000000000000000 ) ) ;
#14549 = CARTESIAN_POINT ( 'NONE',  ( 2.246813503491803310, -4.409619785863921670, -10.34374999795161543 ) ) ;
#14550 = EDGE_LOOP ( 'NONE', ( #5507, #3648 ) ) ;
#14551 = CARTESIAN_POINT ( 'NONE',  ( 17.68117051311639898, -3.372863662543048591, -32.00000000000000000 ) ) ;
#14552 = CARTESIAN_POINT ( 'NONE',  ( 5.699999999999994849, -0.9027913098498966393, -6.500000000000005329 ) ) ;
#14553 = FACE_BOUND ( 'NONE', #12196, .T. ) ;
#14554 = EDGE_CURVE ( 'NONE', #16193, #18731, #11803, .T. ) ;
#14555 = EDGE_LOOP ( 'NONE', ( #10728, #9462 ) ) ;
#14556 = CARTESIAN_POINT ( 'NONE',  ( -2.255998204157477538, -17.85806462366060288, -35.00000000000000000 ) ) ;
#14557 = EDGE_LOOP ( 'NONE', ( #16679, #8373, #16189, #16791 ) ) ;
#14558 = CONTEXT_DEPENDENT_SHAPE_REPRESENTATION ( #34, #8749 ) ;
#14559 = VECTOR ( 'NONE', #8241, 1000.000000000000000 ) ;
#14560 = DIRECTION ( 'NONE',  ( 0.000000000000000000, 0.000000000000000000, 1.000000000000000000 ) ) ;
#14561 = CARTESIAN_POINT ( 'NONE',  ( 0.000000000000000000, 0.000000000000000000, -6.000000000000005329 ) ) ;
#14562 = CARTESIAN_POINT ( 'NONE',  ( 12.32184790671639618, 13.12143529358541016, 32.00000000000000000 ) ) ;
#14563 = EDGE_LOOP ( 'NONE', ( #1715, #18227, #9912, #14462 ) ) ;
#14564 = CARTESIAN_POINT ( 'NONE',  ( 4.644907831421413391, -6.483696736553170581, -2.385244779468109755E-15 ) ) ;
#14565 = CYLINDRICAL_SURFACE ( 'NONE', #15522, 13.19999999999999929 ) ;
#14566 = CYLINDRICAL_SURFACE ( 'NONE', #3755, 3.000000000000000000 ) ;
#14567 = ORIENTED_EDGE ( 'NONE', *, *, #17366, .F. ) ;
#14568 = CARTESIAN_POINT ( 'NONE',  ( 0.1855657389739082119, 5.253342437939721776, 25.39738473785002881 ) ) ;
#14569 = EDGE_CURVE ( 'NONE', #1120, #7944, #19613, .T. ) ;
#14570 = ADVANCED_FACE ( 'NONE', ( #6866 ), #7253, .F. ) ;
#14571 = VERTEX_POINT ( 'NONE', #19476 ) ;
#14572 = AXIS2_PLACEMENT_3D ( 'NONE', #10575, #1266, #12172 ) ;
#14573 = ADVANCED_FACE ( 'NONE', ( #11880 ), #10048, .F. ) ;
#14574 = CARTESIAN_POINT ( 'NONE',  ( 0.000000000000000000, 15.74360496233409634, -18.28042085475261302 ) ) ;
#14575 = DIRECTION ( 'NONE',  ( 0.000000000000000000, 0.000000000000000000, 1.000000000000000000 ) ) ;
#14576 = ORIENTED_EDGE ( 'NONE', *, *, #4793, .T. ) ;
#14577 = CARTESIAN_POINT ( 'NONE',  ( -2.444050593750049849, -4.233219804643852946, -6.468749997951615427 ) ) ;
#14578 = EDGE_CURVE ( 'NONE', #6290, #12336, #9125, .T. ) ;
#14579 = CARTESIAN_POINT ( 'NONE',  ( 0.000000000000000000, 0.000000000000000000, -54.79000000000000625 ) ) ;
#14580 = DIRECTION ( 'NONE',  ( 0.000000000000000000, 0.000000000000000000, 1.000000000000000000 ) ) ;
#14581 = ORIENTED_EDGE ( 'NONE', *, *, #873, .F. ) ;
#14582 = ORIENTED_EDGE ( 'NONE', *, *, #8932, .T. ) ;
#14583 = CARTESIAN_POINT ( 'NONE',  ( 2.789999999999999147, -9.324097380959294412, -22.25075486061747654 ) ) ;
#14584 = VECTOR ( 'NONE', #6923, 1000.000000000000000 ) ;
#14585 = AXIS2_PLACEMENT_3D ( 'NONE', #14544, #5420, #10335 ) ;
#14586 = EDGE_CURVE ( 'NONE', #3731, #13404, #11630, .T. ) ;
#14587 = DIRECTION ( 'NONE',  ( 0.000000000000000000, 0.000000000000000000, -1.000000000000000000 ) ) ;
#14588 = CARTESIAN_POINT ( 'NONE',  ( -1.185096637661215091, 5.575441324182695446, -7.000000000000005329 ) ) ;
#14589 = ORIENTED_EDGE ( 'NONE', *, *, #170, .T. ) ;
#14590 = DIRECTION ( 'NONE',  ( 0.000000000000000000, 0.000000000000000000, 1.000000000000000000 ) ) ;
#14591 = CARTESIAN_POINT ( 'NONE',  ( 10.34374999795161543, 0.2590123213421660631, -4.942249507334554259 ) ) ;
#14592 = ORIENTED_EDGE ( 'NONE', *, *, #7299, .F. ) ;
#14593 = DIRECTION ( 'NONE',  ( 1.000000000000000000, -0.000000000000000000, 0.000000000000000000 ) ) ;
#14594 = ADVANCED_FACE ( 'NONE', ( #7562 ), #15084, .T. ) ;
#14595 =( BOUNDED_SURFACE ( )  B_SPLINE_SURFACE ( 1, 2, ( 
 ( #7774, #13984, #6263, #369, #18578, #4876, #15585, #1874, #14076, #6451, #274, #180, #10884, #12388, #16990, #3272, #37 ),
 ( #10836, #3330, #18727, #8016, #12437, #4729, #15541, #15441, #230, #14232, #3226, #5023, #8126, #537, #17041, #11134, #18631 ) ),
 .UNSPECIFIED., .F., .F., .F. ) 
 B_SPLINE_SURFACE_WITH_KNOTS ( ( 2, 2 ),
 ( 3, 2, 2, 2, 2, 2, 2, 2, 3 ),
 ( 0.000000000000000000, 1.000000000000000000 ),
 ( 0.000000000000000000, 0.05000000000000000278, 0.1000000000000000056, 0.1499999999999999944, 0.2000000000000000111, 0.2500000000000000000, 0.2999999999999999889, 0.3499999999999999778, 0.4000000000000000222 ),
 .UNSPECIFIED. ) 
 GEOMETRIC_REPRESENTATION_ITEM ( )  RATIONAL_B_SPLINE_SURFACE ( (
 ( 1.000000000000000000, 0.9876883405951377704, 1.000000000000000000, 0.9876883405951377704, 1.000000000000000000, 0.9876883405951377704, 1.000000000000000000, 0.9876883405951377704, 1.000000000000000000, 0.9876883405951377704, 1.000000000000000000, 0.9876883405951377704, 1.000000000000000000, 0.9876883405951377704, 1.000000000000000000, 0.9876883405951377704, 1.000000000000000000),
 ( 1.000000000000000000, 0.9876883405951377704, 1.000000000000000000, 0.9876883405951377704, 1.000000000000000000, 0.9876883405951377704, 1.000000000000000000, 0.9876883405951377704, 1.000000000000000000, 0.9876883405951377704, 1.000000000000000000, 0.9876883405951377704, 1.000000000000000000, 0.9876883405951377704, 1.000000000000000000, 0.9876883405951377704, 1.000000000000000000) ) ) 
 REPRESENTATION_ITEM ( '' )  SURFACE ( )  );
#14596 = AXIS2_PLACEMENT_3D ( 'NONE', #5765, #13379, #1382 ) ;
#14597 = CIRCLE ( 'NONE', #13312, 3.000000000000000000 ) ;
#14598 = CARTESIAN_POINT ( 'NONE',  ( -2.500000000000002220, 0.000000000000000000, 0.000000000000000000 ) ) ;
#14599 = CARTESIAN_POINT ( 'NONE',  ( 1.039999999999997149, -27.68468304288261805, 4.633866840648821039 ) ) ;
#14600 = CARTESIAN_POINT ( 'NONE',  ( 12.84374999795161543, -1.016293382781378485, -4.781284448697201483 ) ) ;
#14601 = DIRECTION ( 'NONE',  ( -1.000000000000000000, -0.000000000000000000, -0.000000000000000000 ) ) ;
#14602 = CARTESIAN_POINT ( 'NONE',  ( 3.255998204157476206, -17.85806462366060288, 32.00000000000000000 ) ) ;
#14603 = VERTEX_POINT ( 'NONE', #6060 ) ;
#14604 = DIRECTION ( 'NONE',  ( 0.000000000000000000, 0.000000000000000000, 1.000000000000000000 ) ) ;
#14605 = DIRECTION ( 'NONE',  ( -0.000000000000000000, -0.000000000000000000, 1.000000000000000000 ) ) ;
#14606 = UNCERTAINTY_MEASURE_WITH_UNIT (LENGTH_MEASURE( 1.000000000000000082E-05 ), #9716, 'distance_accuracy_value', 'NONE');
#14607 = CARTESIAN_POINT ( 'NONE',  ( 1.988169868018562880, -4.465502636338038123, -13.84374999795161543 ) ) ;
#14608 = ADVANCED_FACE ( 'NONE', ( #13473 ), #15286, .F. ) ;
#14609 = DIRECTION ( 'NONE',  ( -1.000000000000000000, 1.224646799147353207E-16, 0.000000000000000000 ) ) ;
#14610 = AXIS2_PLACEMENT_3D ( 'NONE', #16199, #8784, #5572 ) ;
#14611 = DIRECTION ( 'NONE',  ( 0.000000000000000000, -0.7315216790650492795, 0.6818181818181815457 ) ) ;
#14612 = VECTOR ( 'NONE', #4706, 1000.000000000000000 ) ;
#14613 = ORIENTED_EDGE ( 'NONE', *, *, #7683, .F. ) ;
#14614 = CARTESIAN_POINT ( 'NONE',  ( 6.843749997951615427, -3.413342815706642518E-14, 4.888101187500000222 ) ) ;
#14615 = DIRECTION ( 'NONE',  ( 1.000000000000000000, 0.000000000000000000, 0.000000000000000000 ) ) ;
#14616 = EDGE_CURVE ( 'NONE', #8799, #15782, #14186, .T. ) ;
#14617 = ORIENTED_EDGE ( 'NONE', *, *, #190, .F. ) ;
#14618 = EDGE_CURVE ( 'NONE', #14637, #11664, #7658, .T. ) ;
#14619 = CARTESIAN_POINT ( 'NONE',  ( 0.1882239080259273667, 5.251266773802727883, -25.40949241676348080 ) ) ;
#14620 = PLANE ( 'NONE',  #19544 ) ;
#14621 = CARTESIAN_POINT ( 'NONE',  ( 6.843749997951615427, 4.233219804643871598, 2.444050593750020095 ) ) ;
#14622 = ORIENTED_EDGE ( 'NONE', *, *, #8356, .F. ) ;
#14623 = CIRCLE ( 'NONE', #13022, 28.06981291497571362 ) ;
#14624 = DIRECTION ( 'NONE',  ( 0.000000000000000000, 0.000000000000000000, -1.000000000000000000 ) ) ;
#14625 = SURFACE_STYLE_USAGE ( .BOTH. , #13114 ) ;
#14626 = DIRECTION ( 'NONE',  ( 0.000000000000000000, 0.000000000000000000, 1.000000000000000000 ) ) ;
#14627 = CIRCLE ( 'NONE', #13663, 28.06981291497571007 ) ;
#14628 = DIRECTION ( 'NONE',  ( -1.000000000000000000, -0.000000000000000000, -0.000000000000000000 ) ) ;
#14629 = ORIENTED_EDGE ( 'NONE', *, *, #8678, .F. ) ;
#14630 = LINE ( 'NONE', #3913, #10481 ) ;
#14631 = EDGE_LOOP ( 'NONE', ( #16319, #13128, #9771, #7044, #15711 ) ) ;
#14632 = CARTESIAN_POINT ( 'NONE',  ( 2.031033471609898111, 3.797536611356316705, 27.31260702007176988 ) ) ;
#14633 = CARTESIAN_POINT ( 'NONE',  ( 3.350375938067096548, 4.611396867937201272, -14.31249999590322552 ) ) ;
#14634 = EDGE_CURVE ( 'NONE', #11459, #7744, #3652, .T. ) ;
#14635 = CYLINDRICAL_SURFACE ( 'NONE', #4834, 1.000000000000004441 ) ;
#14636 = DIRECTION ( 'NONE',  ( -1.000000000000000000, 0.000000000000000000, 0.000000000000000000 ) ) ;
#14637 = VERTEX_POINT ( 'NONE', #10776 ) ;
#14638 = CARTESIAN_POINT ( 'NONE',  ( 2.601776096565022289, 12.84621645676845070, 22.54313264455018384 ) ) ;
#14639 = DIRECTION ( 'NONE',  ( -1.000000000000000000, 1.224646799147353207E-16, 0.000000000000000000 ) ) ;
#14640 = VECTOR ( 'NONE', #10396, 1000.000000000000000 ) ;
#14641 = EDGE_LOOP ( 'NONE', ( #14467, #16976, #2487, #17945 ) ) ;
#14642 = EDGE_CURVE ( 'NONE', #9172, #14916, #5866, .T. ) ;
#14643 = AXIS2_PLACEMENT_3D ( 'NONE', #3504, #18703, #5195 ) ;
#14644 = CARTESIAN_POINT ( 'NONE',  ( 2.789999999999999147, 23.31896751603342821, -7.334849878007252855 ) ) ;
#14645 = CARTESIAN_POINT ( 'NONE',  ( -2.620002426024580000, -5.142044285764733935, -13.81249999590322552 ) ) ;
#14646 = ORIENTED_EDGE ( 'NONE', *, *, #12816, .F. ) ;
#14647 = DIRECTION ( 'NONE',  ( 0.000000000000000000, 0.000000000000000000, -1.000000000000000000 ) ) ;
#14648 = EDGE_CURVE ( 'NONE', #7726, #4563, #2399, .T. ) ;
#14649 = CARTESIAN_POINT ( 'NONE',  ( 5.421022142882364392, -1.761396867937238486, -7.000000000000005329 ) ) ;
#14650 = PLANE ( 'NONE',  #13874 ) ;
#14651 = VERTEX_POINT ( 'NONE', #12085 ) ;
#14652 = DIRECTION ( 'NONE',  ( -0.000000000000000000, -0.000000000000000000, 1.000000000000000000 ) ) ;
#14653 = CIRCLE ( 'NONE', #2491, 4.400000000000000355 ) ;
#14654 = ORIENTED_EDGE ( 'NONE', *, *, #6666, .T. ) ;
#14655 = CIRCLE ( 'NONE', #8891, 8.265000000000021885 ) ;
#14656 =( NAMED_UNIT ( * ) SI_UNIT ( $, .STERADIAN. ) SOLID_ANGLE_UNIT ( ) );
#14657 = DIRECTION ( 'NONE',  ( 0.000000000000000000, 0.000000000000000000, -1.000000000000000000 ) ) ;
#14658 = ORIENTED_EDGE ( 'NONE', *, *, #16149, .T. ) ;
#14659 = CARTESIAN_POINT ( 'NONE',  ( -3.383411828340740850E-14, -4.888101187500000222, -11.84374999795161365 ) ) ;
#14660 = CARTESIAN_POINT ( 'NONE',  ( 13.00000000000000000, -5.567819778318897406, -1.220402768007724292 ) ) ;
#14661 = CARTESIAN_POINT ( 'NONE',  ( 18.11901729331276911, 5.562305898749055011, -35.00000000000000000 ) ) ;
#14662 = ORIENTED_EDGE ( 'NONE', *, *, #2059, .T. ) ;
#14663 = EDGE_CURVE ( 'NONE', #16676, #8648, #3445, .T. ) ;
#14664 = FACE_OUTER_BOUND ( 'NONE', #1748, .T. ) ;
#14665 = PRODUCT_DEFINITION_SHAPE ( 'NONE', 'NONE',  #19800 ) ;
#14666 = AXIS2_PLACEMENT_3D ( 'NONE', #7215, #14848, #13434 ) ;
#14667 = ORIENTED_EDGE ( 'NONE', *, *, #4243, .T. ) ;
#14668 = CARTESIAN_POINT ( 'NONE',  ( 2.718184749312774873, 25.22524549359950541, 2.576941577947493567 ) ) ;
#14669 = COLOUR_RGB ( '', 0.72549020, 0.75294118, 0.79215686) ;
#14670 = CARTESIAN_POINT ( 'NONE',  ( 1.039999999999996705, 27.76164181293051669, -4.147968289691385202 ) ) ;
#14671 = ORIENTED_EDGE ( 'NONE', *, *, #17717, .T. ) ;
#14672 = CARTESIAN_POINT ( 'NONE',  ( 7.468749997951615427, -4.781284448697200595, 1.016293382781377819 ) ) ;
#14673 = DIRECTION ( 'NONE',  ( 1.000000000000000000, 0.000000000000000000, 0.000000000000000000 ) ) ;
#14674 = EDGE_CURVE ( 'NONE', #736, #12976, #15764, .T. ) ;
#14675 = ORIENTED_EDGE ( 'NONE', *, *, #3216, .F. ) ;
#14676 = EDGE_CURVE ( 'NONE', #16711, #4579, #1073, .T. ) ;
#14677 = EDGE_CURVE ( 'NONE', #3117, #3527, #6253, .T. ) ;
#14678 = ORIENTED_EDGE ( 'NONE', *, *, #2920, .T. ) ;
#14679 = CARTESIAN_POINT ( 'NONE',  ( -5.700000000000001954, 6.980486755139915080E-16, 0.000000000000000000 ) ) ;
#14680 = AXIS2_PLACEMENT_3D ( 'NONE', #1156, #2642, #2540 ) ;
#14681 = FACE_OUTER_BOUND ( 'NONE', #14641, .T. ) ;
#14682 = CYLINDRICAL_SURFACE ( 'NONE', #10497, 5.700000000000001954 ) ;
#14683 = EDGE_LOOP ( 'NONE', ( #8993, #16362, #4701, #10510 ) ) ;
#14684 = EDGE_CURVE ( 'NONE', #17509, #19081, #15190, .T. ) ;
#14685 = EDGE_CURVE ( 'NONE', #5172, #9689, #4471, .T. ) ;
#14686 = DIRECTION ( 'NONE',  ( 1.000000000000000000, 0.000000000000000000, 0.000000000000000000 ) ) ;
#14687 = CARTESIAN_POINT ( 'NONE',  ( 7.843749997951614539, -3.270778111535287191, -3.632567103900569361 ) ) ;
#14688 = ORIENTED_EDGE ( 'NONE', *, *, #13868, .T. ) ;
#14689 = CARTESIAN_POINT ( 'NONE',  ( 0.02436607992775978102, 2.336989772644613161, -24.63872515616080250 ) ) ;
#14690 = CARTESIAN_POINT ( 'NONE',  ( 1.394999999999998685, 19.67366047555559661, -20.02152543075324331 ) ) ;
#14691 = CARTESIAN_POINT ( 'NONE',  ( -3.968750000000007994, -6.874076642538976323, 0.000000000000000000 ) ) ;
#14692 = DIRECTION ( 'NONE',  ( -1.000000000000000000, 0.000000000000000000, 0.000000000000000000 ) ) ;
#14693 = CIRCLE ( 'NONE', #5427, 4.500000000000000000 ) ;
#14694 = CARTESIAN_POINT ( 'NONE',  ( 1.886022603841296608, 0.000000000000000000, 0.000000000000000000 ) ) ;
#14695 = CARTESIAN_POINT ( 'NONE',  ( -5.476417968967388639, 17.43449690031536292, 32.00000000000000000 ) ) ;
#14696 = EDGE_LOOP ( 'NONE', ( #8412, #5108 ) ) ;
#14697 = CARTESIAN_POINT ( 'NONE',  ( 1.545624935189822177E-15, 9.165435523385314198, -6.527800000000000047 ) ) ;
#14698 = CARTESIAN_POINT ( 'NONE',  ( 1.039999999999997593, 0.000000000000000000, 0.000000000000000000 ) ) ;
#14699 = CARTESIAN_POINT ( 'NONE',  ( 0.5958122406255995651, -5.668774803599162304, -15.31249999590322552 ) ) ;
#14700 = CARTESIAN_POINT ( 'NONE',  ( 4.465502636338039011, 1.988169868018562436, -8.468749997951615427 ) ) ;
#14701 = CARTESIAN_POINT ( 'NONE',  ( -36.00000000000000000, -4.400000000000000355, 5.388445916248354013E-16 ) ) ;
#14702 = ORIENTED_EDGE ( 'NONE', *, *, #14569, .T. ) ;
#14703 = EDGE_CURVE ( 'NONE', #2600, #993, #18711, .T. ) ;
#14704 = CARTESIAN_POINT ( 'NONE',  ( 2.783068961317271217, -12.53626894672843051, 21.08061549536610713 ) ) ;
#14705 =( BOUNDED_CURVE ( )  B_SPLINE_CURVE ( 2, ( #15934, #3725, #4017, #8616, #3820, #16323, #13225, #6809, #2603, #14821, #5220, #14434, #9845, #10129, #14633, #2317, #732 ),
 .UNSPECIFIED., .F., .F. ) 
 B_SPLINE_CURVE_WITH_KNOTS ( ( 3, 2, 2, 2, 2, 2, 2, 2, 3 ),
 ( 0.000000000000000000, 0.05000000000000000971, 0.1000000000000000194, 0.1499999999999999944, 0.2000000000000000389, 0.2500000000000000000, 0.2999999999999999889, 0.3499999999999999223, 0.4000000000000000777 ),
 .UNSPECIFIED. ) 
 CURVE ( )  GEOMETRIC_REPRESENTATION_ITEM ( )  RATIONAL_B_SPLINE_CURVE ( ( 1.000000000000000000, 0.9876883405951377704, 1.000000000000000000, 0.9876883405951377704, 1.000000000000000000, 0.9876883405951377704, 1.000000000000000000, 0.9876883405951377704, 1.000000000000000000, 0.9876883405951377704, 1.000000000000000000, 0.9876883405951377704, 1.000000000000000000, 0.9876883405951377704, 1.000000000000000000, 0.9876883405951377704, 1.000000000000000000 ) ) 
 REPRESENTATION_ITEM ( '' )  );
#14706 = EDGE_CURVE ( 'NONE', #13582, #6761, #14180, .T. ) ;
#14707 = CARTESIAN_POINT ( 'NONE',  ( 2.789999999999999147, -1.991882183130462503, 24.04302995059964942 ) ) ;
#14708 = COLOUR_RGB ( '', 0.31764706, 0.68627451, 0.89019608) ;
#14709 = ORIENTED_EDGE ( 'NONE', *, *, #16725, .F. ) ;
#14710 = FACE_OUTER_BOUND ( 'NONE', #4118, .T. ) ;
#14711 = VECTOR ( 'NONE', #7512, 1000.000000000000000 ) ;
#14712 = CARTESIAN_POINT ( 'NONE',  ( -5.209999999999999964, 0.000000000000000000, 0.000000000000000000 ) ) ;
#14713 = DIRECTION ( 'NONE',  ( 0.000000000000000000, 1.000000000000000000, 0.000000000000000000 ) ) ;
#14714 = ADVANCED_FACE ( 'NONE', ( #17178, #18767 ), #12774, .F. ) ;
#14715 = ORIENTED_EDGE ( 'NONE', *, *, #18190, .T. ) ;
#14716 = CARTESIAN_POINT ( 'NONE',  ( 11.32184790671639263, 13.12143529358541016, 32.00000000000000000 ) ) ;
#14717 =( LENGTH_UNIT ( ) NAMED_UNIT ( * ) SI_UNIT ( .MILLI., .METRE. ) );
#14718 = CARTESIAN_POINT ( 'NONE',  ( 3.632567103900546712, 3.270778111535313837, -7.843749997951614539 ) ) ;
#14719 = CYLINDRICAL_SURFACE ( 'NONE', #15355, 6.000000000000000000 ) ;
#14720 = VERTEX_POINT ( 'NONE', #4867 ) ;
#14721 = DIRECTION ( 'NONE',  ( 0.000000000000000000, -1.000000000000000000, 0.000000000000000000 ) ) ;
#14722 = VERTEX_POINT ( 'NONE', #9785 ) ;
#14723 = AXIS2_PLACEMENT_3D ( 'NONE', #16521, #7595, #2896 ) ;
#14724 = EDGE_CURVE ( 'NONE', #8429, #19636, #17760, .T. ) ;
#14725 = FACE_OUTER_BOUND ( 'NONE', #4517, .T. ) ;
#14726 = CARTESIAN_POINT ( 'NONE',  ( -2.000000000000000000, -8.000000000000003553, 41.99999999999999289 ) ) ;
#14727 = CARTESIAN_POINT ( 'NONE',  ( 8.000000000000000000, 0.000000000000000000, 0.000000000000000000 ) ) ;
#14728 = CARTESIAN_POINT ( 'NONE',  ( 2.500000000000002220, 0.000000000000000000, 0.000000000000000000 ) ) ;
#14729 = EDGE_LOOP ( 'NONE', ( #1488, #11663, #12038, #10595 ) ) ;
#14730 = CARTESIAN_POINT ( 'NONE',  ( -2.000000000000001776, 0.000000000000000000, 0.000000000000000000 ) ) ;
#14731 = DIRECTION ( 'NONE',  ( 0.000000000000000000, 0.000000000000000000, -1.000000000000000000 ) ) ;
#14732 = ORIENTED_EDGE ( 'NONE', *, *, #17045, .F. ) ;
#14733 = AXIS2_PLACEMENT_3D ( 'NONE', #18589, #9402, #3388 ) ;
#14734 =( REPRESENTATION_RELATIONSHIP ('NONE','NONE', #18211, #4652 ) REPRESENTATION_RELATIONSHIP_WITH_TRANSFORMATION ( #9321 )SHAPE_REPRESENTATION_RELATIONSHIP( ) );
#14735 = EDGE_CURVE ( 'NONE', #13251, #15913, #11647, .T. ) ;
#14736 = CARTESIAN_POINT ( 'NONE',  ( 2.789999999999999147, 0.000000000000000000, 0.000000000000000000 ) ) ;
#14737 = CARTESIAN_POINT ( 'NONE',  ( 2.765633920072242180, 22.71065055754465689, -9.836394144775473691 ) ) ;
#14738 = ORIENTED_EDGE ( 'NONE', *, *, #4174, .F. ) ;
#14739 = DIRECTION ( 'NONE',  ( -1.000000000000000000, 0.000000000000000000, 0.000000000000000000 ) ) ;
#14740 = CARTESIAN_POINT ( 'NONE',  ( -13.86923836996420967, -11.47363181547641275, 32.00000000000000000 ) ) ;
#14741 = FACE_BOUND ( 'NONE', #13027, .T. ) ;
#14742 = ORIENTED_EDGE ( 'NONE', *, *, #16665, .F. ) ;
#14743 = FACE_OUTER_BOUND ( 'NONE', #3325, .T. ) ;
#14744 = ORIENTED_EDGE ( 'NONE', *, *, #16802, .F. ) ;
#14745 = CYLINDRICAL_SURFACE ( 'NONE', #9176, 13.19999999999999929 ) ;
#14746 = EDGE_LOOP ( 'NONE', ( #6293, #16244, #5541, #15046 ) ) ;
#14747 = DIRECTION ( 'NONE',  ( 0.000000000000000000, 1.000000000000000000, -1.224646799147353207E-16 ) ) ;
#14748 = DIRECTION ( 'NONE',  ( -0.1045284632676491549, 0.9945218953682738450, 0.000000000000000000 ) ) ;
#14749 = CARTESIAN_POINT ( 'NONE',  ( 2.255998204157473097, -17.85806462366060288, 35.00000000000000000 ) ) ;
#14750 = ORIENTED_EDGE ( 'NONE', *, *, #12990, .F. ) ;
#14751 = CARTESIAN_POINT ( 'NONE',  ( -3.383411828340740850E-14, -4.888101187500000222, -11.46874999795161543 ) ) ;
#14752 = CARTESIAN_POINT ( 'NONE',  ( 13.50000000000000533, 1.493657965219562067, -5.574407415329146964 ) ) ;
#14753 = AXIS2_PLACEMENT_3D ( 'NONE', #17856, #4151, #5837 ) ;
#14754 = CARTESIAN_POINT ( 'NONE',  ( 2.999999999999998224, 3.950217066951266176, 3.681818181818181213 ) ) ;
#14755 = ORIENTED_EDGE ( 'NONE', *, *, #6322, .T. ) ;
#14756 = CIRCLE ( 'NONE', #19517, 9.000000000000000000 ) ;
#14757 = DIRECTION ( 'NONE',  ( 0.000000000000000000, 0.000000000000000000, -1.000000000000000000 ) ) ;
#14758 = VERTEX_POINT ( 'NONE', #3466 ) ;
#14759 = CIRCLE ( 'NONE', #8686, 6.500000000000000000 ) ;
#14760 = AXIS2_PLACEMENT_3D ( 'NONE', #18585, #17093, #6176 ) ;
#14761 = CARTESIAN_POINT ( 'NONE',  ( 2.765633920072235963, 24.63872515616082737, 2.336989772644355146 ) ) ;
#14762 = CIRCLE ( 'NONE', #19536, 24.12539914357697413 ) ;
#14763 = CARTESIAN_POINT ( 'NONE',  ( 2.255998204157473097, -17.85806462366060288, 32.00000000000000000 ) ) ;
#14764 = ORIENTED_EDGE ( 'NONE', *, *, #1827, .F. ) ;
#14765 = DIRECTION ( 'NONE',  ( 0.000000000000000000, 0.000000000000000000, 1.000000000000000000 ) ) ;
#14766 = DIRECTION ( 'NONE',  ( 0.000000000000000000, 0.000000000000000000, 1.000000000000000000 ) ) ;
#14767 = EDGE_CURVE ( 'NONE', #12820, #10790, #3011, .T. ) ;
#14768 = AXIS2_PLACEMENT_3D ( 'NONE', #17692, #2284, #5475 ) ;
#14769 = ORIENTED_EDGE ( 'NONE', *, *, #8843, .F. ) ;
#14770 = ORIENTED_EDGE ( 'NONE', *, *, #7936, .F. ) ;
#14771 = CARTESIAN_POINT ( 'NONE',  ( 8.671566133830875600, 15.77352024078954784, 32.00000000000000000 ) ) ;
#14772 = CARTESIAN_POINT ( 'NONE',  ( 6.500000000000005329, 4.484949146646356688, 3.631840208645826795 ) ) ;
#14773 = ORIENTED_EDGE ( 'NONE', *, *, #5666, .T. ) ;
#14774 = VECTOR ( 'NONE', #1403, 1000.000000000000000 ) ;
#14775 = CYLINDRICAL_SURFACE ( 'NONE', #15524, 4.000000000000000000 ) ;
#14776 = CIRCLE ( 'NONE', #5807, 9.000000000000000000 ) ;
#14777 = ORIENTED_EDGE ( 'NONE', *, *, #4351, .T. ) ;
#14778 = CARTESIAN_POINT ( 'NONE',  ( 1.000000000000003331, 18.00000000000000355, -32.00000000000000000 ) ) ;
#14779 = CIRCLE ( 'NONE', #11577, 6.735000000000022524 ) ;
#14780 = CARTESIAN_POINT ( 'NONE',  ( 8.312499995903225525, -3.814044456245443193, -4.235925505221191933 ) ) ;
#14781 = ORIENTED_EDGE ( 'NONE', *, *, #11268, .T. ) ;
#14782 = DIRECTION ( 'NONE',  ( 0.000000000000000000, 0.000000000000000000, -1.000000000000000000 ) ) ;
#14783 = VECTOR ( 'NONE', #5264, 1000.000000000000000 ) ;
#14784 = ADVANCED_FACE ( 'NONE', ( #360, #12675, #16981, #15673, #574, #6645, #8164, #9576, #10975, #5061, #18869, #6444, #17270, #7955, #5153, #3264, #9380, #1769, #15576, #264, #1962, #3660, #3368, #6348, #8057, #17078, #9479 ), #1866, .F. ) ;
#14785 = CYLINDRICAL_SURFACE ( 'NONE', #4875, 1.000000000000002665 ) ;
#14786 = CARTESIAN_POINT ( 'NONE',  ( -4.644907831421410727, 6.483696736553158146, 4.577366046962239032E-15 ) ) ;
#14787 = DIRECTION ( 'NONE',  ( -1.000000000000000000, 0.000000000000000000, -0.000000000000000000 ) ) ;
#14788 = CIRCLE ( 'NONE', #15423, 0.9999999999999974465 ) ;
#14789 = DIRECTION ( 'NONE',  ( 0.000000000000000000, 0.000000000000000000, 1.000000000000000000 ) ) ;
#14790 =( NAMED_UNIT ( * ) SI_UNIT ( $, .STERADIAN. ) SOLID_ANGLE_UNIT ( ) );
#14791 = CARTESIAN_POINT ( 'NONE',  ( -7.664413047240269201E-14, 2.133839912090805147, 24.22524813288763568 ) ) ;
#14792 = EDGE_CURVE ( 'NONE', #3914, #9386, #2676, .T. ) ;
#14793 = ORIENTED_EDGE ( 'NONE', *, *, #4939, .F. ) ;
#14794 = DIRECTION ( 'NONE',  ( 0.000000000000000000, 0.000000000000000000, 1.000000000000000000 ) ) ;
#14795 = CARTESIAN_POINT ( 'NONE',  ( 5.700000000000002842, 9.001153973733047589E-16, -18.00000000000000355 ) ) ;
#14796 = CIRCLE ( 'NONE', #6793, 4.400000000000000355 ) ;
#14797 = UNCERTAINTY_MEASURE_WITH_UNIT (LENGTH_MEASURE( 1.000000000000000082E-05 ), #9869, 'distance_accuracy_value', 'NONE');
#14798 = LINE ( 'NONE', #19287, #4486 ) ;
#14799 = CIRCLE ( 'NONE', #16398, 28.06981291497571007 ) ;
#14800 = CARTESIAN_POINT ( 'NONE',  ( 0.5109457054261454800, -4.861323657744410554, -14.46874999795161720 ) ) ;
#14801 = CARTESIAN_POINT ( 'NONE',  ( -4.233219804643904460, -2.444050593749961031, -11.84374999795161365 ) ) ;
#14802 = B_SPLINE_CURVE_WITH_KNOTS ( 'NONE', 3,
 ( #12650, #11147, #12947, #14737 ),
 .UNSPECIFIED., .F., .F.,
 ( 4, 4 ),
 ( 0.005258105385878691744, 0.005948373736081389272 ),
 .UNSPECIFIED. ) ;
#14803 = EDGE_LOOP ( 'NONE', ( #1006, #5811 ) ) ;
#14804 = CARTESIAN_POINT ( 'NONE',  ( 2.790000000000079527, -18.34439787333494820, -15.96555658743782580 ) ) ;
#14805 = CARTESIAN_POINT ( 'NONE',  ( 2.765633920072235519, 18.55949924794892780, 16.37294372382865504 ) ) ;
#14806 = ORIENTED_EDGE ( 'NONE', *, *, #1499, .T. ) ;
#14807 = DIRECTION ( 'NONE',  ( 1.000000000000000000, 0.000000000000000000, 0.000000000000000000 ) ) ;
#14808 = ADVANCED_FACE ( 'NONE', ( #15972 ), #10169, .F. ) ;
#14809 = CARTESIAN_POINT ( 'NONE',  ( 2.601776091974069338, 5.251266773802368171, 25.40949241676355541 ) ) ;
#14810 = FACE_OUTER_BOUND ( 'NONE', #7257, .T. ) ;
#14811 = LINE ( 'NONE', #2305, #449 ) ;
#14812 = EDGE_CURVE ( 'NONE', #2723, #10856, #10693, .T. ) ;
#14813 = ORIENTED_EDGE ( 'NONE', *, *, #14642, .F. ) ;
#14814 = LINE ( 'NONE', #10319, #4364 ) ;
#14815 = CARTESIAN_POINT ( 'NONE',  ( 7.312499995903225525, -3.980288726281172656E-14, 5.700000000000001066 ) ) ;
#14816 = ORIENTED_EDGE ( 'NONE', *, *, #9573, .F. ) ;
#14817 = EDGE_CURVE ( 'NONE', #10168, #10294, #18664, .T. ) ;
#14818 = CARTESIAN_POINT ( 'NONE',  ( 2.789999999999999147, -7.909232158574988958, 24.34211360614297348 ) ) ;
#14819 = ORIENTED_EDGE ( 'NONE', *, *, #18491, .T. ) ;
#14820 = CARTESIAN_POINT ( 'NONE',  ( -1.300631254478304744, 8.414515718495824359, -0.3148715423363414589 ) ) ;
#14821 = CARTESIAN_POINT ( 'NONE',  ( -0.9027913098498572264, 5.700000000000000178, -11.81249999590322552 ) ) ;
#14822 = PRODUCT_DEFINITION_SHAPE ( 'NONE', 'NONE',  #19787 ) ;
#14823 = DIRECTION ( 'NONE',  ( 0.000000000000000000, 0.000000000000000000, 1.000000000000000000 ) ) ;
#14824 = CARTESIAN_POINT ( 'NONE',  ( 2.620002426024544029, 5.142044285764751699, -12.50000000000000533 ) ) ;
#14825 = VERTEX_POINT ( 'NONE', #5647 ) ;
#14826 = CARTESIAN_POINT ( 'NONE',  ( -4.233219804643904460, -2.444050593749961031, -11.46874999795161543 ) ) ;
#14827 = ADVANCED_FACE ( 'NONE', ( #11760 ), #17864, .T. ) ;
#14828 = CARTESIAN_POINT ( 'NONE',  ( 0.000000000000000000, 0.000000000000000000, -35.00000000000000000 ) ) ;
#14829 = ORIENTED_EDGE ( 'NONE', *, *, #16877, .F. ) ;
#14830 = VECTOR ( 'NONE', #18949, 1000.000000000000000 ) ;
#14831 = EDGE_CURVE ( 'NONE', #3527, #10068, #8762, .T. ) ;
#14832 = CARTESIAN_POINT ( 'NONE',  ( 1.886022603841227330, 0.000000000000000000, 0.000000000000000000 ) ) ;
#14833 = CARTESIAN_POINT ( 'NONE',  ( 2.789999999999999147, 0.000000000000000000, 0.000000000000000000 ) ) ;
#14834 = B_SPLINE_CURVE_WITH_KNOTS ( 'NONE', 3,
 ( #12684, #12783, #1876, #18775, #2169, #8376, #14078, #18880, #14492, #9893 ),
 .UNSPECIFIED., .F., .F.,
 ( 4, 3, 3, 4 ),
 ( 0.000000000000000000, 0.0001875345074742620726, 0.0003808595644229701067, 0.0005744879655065565855 ),
 .UNSPECIFIED. ) ;
#14835 = ORIENTED_EDGE ( 'NONE', *, *, #8490, .F. ) ;
#14836 = CARTESIAN_POINT ( 'NONE',  ( 3.631840208645826795, 4.484949146646356688, -6.500000000000005329 ) ) ;
#14837 = DIRECTION ( 'NONE',  ( -0.9238795325112865164, -0.3826834323650906700, 0.000000000000000000 ) ) ;
#14838 = CARTESIAN_POINT ( 'NONE',  ( 12.84374999795161543, -3.632567103900546712, 3.270778111535314281 ) ) ;
#14839 = ORIENTED_EDGE ( 'NONE', *, *, #10828, .F. ) ;
#14840 = DIRECTION ( 'NONE',  ( -1.000000000000000000, -0.000000000000000000, -0.000000000000000000 ) ) ;
#14841 = ORIENTED_EDGE ( 'NONE', *, *, #8569, .F. ) ;
#14842 = CARTESIAN_POINT ( 'NONE',  ( 0.000000000000000000, 0.000000000000000000, 0.000000000000000000 ) ) ;
#14843 = VERTEX_POINT ( 'NONE', #12871 ) ;
#14844 = ADVANCED_FACE ( 'NONE', ( #16363 ), #6158, .T. ) ;
#14845 = DIRECTION ( 'NONE',  ( 0.000000000000000000, 1.224646799147353454E-16, 1.000000000000000000 ) ) ;
#14846 = DIRECTION ( 'NONE',  ( -0.000000000000000000, -0.7315216790650492795, -0.6818181818181815457 ) ) ;
#14847 = CARTESIAN_POINT ( 'NONE',  ( 1.799999999999999600, 0.000000000000000000, -4.000000000000000000 ) ) ;
#14848 = DIRECTION ( 'NONE',  ( -1.000000000000000000, -0.000000000000000000, -0.000000000000000000 ) ) ;
#14849 = CYLINDRICAL_SURFACE ( 'NONE', #6552, 1.000000000000000888 ) ;
#14850 = AXIS2_PLACEMENT_3D ( 'NONE', #10757, #8861, #5741 ) ;
#14851 = DIRECTION ( 'NONE',  ( -1.000000000000000000, -0.000000000000000000, -0.000000000000000000 ) ) ;
#14852 = ORIENTED_EDGE ( 'NONE', *, *, #8769, .F. ) ;
#14853 = EDGE_CURVE ( 'NONE', #13643, #11673, #12960, .T. ) ;
#14854 = CARTESIAN_POINT ( 'NONE',  ( -12.32184790671639085, 13.12143529358541549, -32.00000000000000000 ) ) ;
#14855 = CIRCLE ( 'NONE', #13898, 1.000000000000002665 ) ;
#14856 = EDGE_CURVE ( 'NONE', #488, #6321, #16128, .T. ) ;
#14857 = ORIENTED_EDGE ( 'NONE', *, *, #19583, .F. ) ;
#14858 = CARTESIAN_POINT ( 'NONE',  ( 0.000000000000000000, 0.000000000000000000, -32.00000000000000000 ) ) ;
#14859 = AXIS2_PLACEMENT_3D ( 'NONE', #15049, #7730, #4638 ) ;
#14860 = PLANE ( 'NONE',  #19505 ) ;
#14861 = LINE ( 'NONE', #5354, #4127 ) ;
#14862 = DIRECTION ( 'NONE',  ( 0.000000000000000000, 0.000000000000000000, -1.000000000000000000 ) ) ;
#14863 = VERTEX_POINT ( 'NONE', #7330 ) ;
#14864 = CARTESIAN_POINT ( 'NONE',  ( -3.632567103900569361, -3.270778111535287191, -7.468749997951615427 ) ) ;
#14865 = CARTESIAN_POINT ( 'NONE',  ( 0.000000000000000000, 0.000000000000000000, -31.00000000000000000 ) ) ;
#14866 = PLANE ( 'NONE',  #9363 ) ;
#14867 = LINE ( 'NONE', #19455, #3533 ) ;
#14868 = EDGE_LOOP ( 'NONE', ( #13171, #5457, #6723, #12672 ) ) ;
#14869 = ORIENTED_EDGE ( 'NONE', *, *, #8974, .T. ) ;
#14870 = CARTESIAN_POINT ( 'NONE',  ( -4.476417968967385974, 17.43449690031536292, -32.00000000000000000 ) ) ;
#14871 = CARTESIAN_POINT ( 'NONE',  ( 8.500000000000007105, 1.493657965219485018, 5.574407415329170057 ) ) ;
#14872 = ORIENTED_EDGE ( 'NONE', *, *, #11467, .T. ) ;
#14873 = AXIS2_PLACEMENT_3D ( 'NONE', #12889, #12790, #18986 ) ;
#14874 = CARTESIAN_POINT ( 'NONE',  ( 0.000000000000000000, -5.535312321042921369, 23.48180575137728354 ) ) ;
#14875 = ORIENTED_EDGE ( 'NONE', *, *, #11015, .F. ) ;
#14876 = CIRCLE ( 'NONE', #14265, 4.824999999999999289 ) ;
#14877 = DIRECTION ( 'NONE',  ( 0.000000000000000000, 0.000000000000000000, 1.000000000000000000 ) ) ;
#14878 = SHAPE_REPRESENTATION ( 'CLUTCH CONE', ( #16724 ), #12592 ) ;
#14879 = CARTESIAN_POINT ( 'NONE',  ( 0.7589665326895889130, -12.98167595241004335, -24.32849926382764849 ) ) ;
#14880 = VERTEX_POINT ( 'NONE', #18262 ) ;
#14881 = LINE ( 'NONE', #5757, #179 ) ;
#14882 = ADVANCED_FACE ( 'NONE', ( #15060 ), #2943, .F. ) ;
#14883 = B_SPLINE_CURVE_WITH_KNOTS ( 'NONE', 3,
 ( #1439, #6124, #1336, #5927, #16750, #7521 ),
 .UNSPECIFIED., .F., .F.,
 ( 4, 2, 4 ),
 ( 2.321268216997094965E-07, 0.001878622960950499009, 0.003757013795079297992 ),
 .UNSPECIFIED. ) ;
#14884 = DIRECTION ( 'NONE',  ( 0.000000000000000000, -1.000000000000000000, 0.000000000000000000 ) ) ;
#14885 = CARTESIAN_POINT ( 'NONE',  ( 12.81249999590322552, 5.699999999999999289, 0.9027913098498566713 ) ) ;
#14886 = CARTESIAN_POINT ( 'NONE',  ( 10.84374999795161543, -3.632567103900500971, -3.270778111535363131 ) ) ;
#14887 = AXIS2_PLACEMENT_3D ( 'NONE', #9540, #9339, #133 ) ;
#14888 = EDGE_CURVE ( 'NONE', #17046, #1346, #7028, .T. ) ;
#14889 = CARTESIAN_POINT ( 'NONE',  ( 1.394999999999998685, 20.02152543075374425, -19.67366047555508857 ) ) ;
#14890 = SHAPE_REPRESENTATION_RELATIONSHIP ( 'NONE' , 'NONE' ,  #14878, #7808 ) ;
#14891 = DIRECTION ( 'NONE',  ( -1.000000000000000000, 0.000000000000000000, 0.000000000000000000 ) ) ;
#14892 = ORIENTED_EDGE ( 'NONE', *, *, #16236, .F. ) ;
#14893 = DIRECTION ( 'NONE',  ( 0.000000000000000000, 0.000000000000000000, 1.000000000000000000 ) ) ;
#14894 = CARTESIAN_POINT ( 'NONE',  ( 2.999999999999998224, 0.000000000000000000, 0.000000000000000000 ) ) ;
#14895 = DIRECTION ( 'NONE',  ( 0.000000000000000000, 0.000000000000000000, 1.000000000000000000 ) ) ;
#14896 = CARTESIAN_POINT ( 'NONE',  ( 0.6476140635210377861, -8.791535369480467210, -0.4930775504667766485 ) ) ;
#14897 = DIRECTION ( 'NONE',  ( -1.000000000000000000, 0.000000000000000000, 0.000000000000000000 ) ) ;
#14898 = ORIENTED_EDGE ( 'NONE', *, *, #10838, .F. ) ;
#14899 = CARTESIAN_POINT ( 'NONE',  ( 2.790000000000000480, -12.51294990530030837, 20.85230829256849105 ) ) ;
#14900 = DIRECTION ( 'NONE',  ( 0.000000000000000000, 0.000000000000000000, 1.000000000000000000 ) ) ;
#14901 = AXIS2_PLACEMENT_3D ( 'NONE', #11329, #11515, #3908 ) ;
#14902 = ORIENTED_EDGE ( 'NONE', *, *, #12335, .F. ) ;
#14903 = DIRECTION ( 'NONE',  ( 1.000000000000000000, 0.000000000000000000, 0.000000000000000000 ) ) ;
#14904 = EDGE_CURVE ( 'NONE', #4439, #11113, #8256, .T. ) ;
#14905 = VECTOR ( 'NONE', #5564, 1000.000000000000000 ) ;
#14906 = CARTESIAN_POINT ( 'NONE',  ( 8.000000000000000000, 0.000000000000000000, 0.000000000000000000 ) ) ;
#14907 = CARTESIAN_POINT ( 'NONE',  ( 2.765633920072239516, -24.63872515616084513, 2.336989772644183283 ) ) ;
#14908 = DIRECTION ( 'NONE',  ( -1.000000000000000000, 0.000000000000000000, 0.000000000000000000 ) ) ;
#14909 = ORIENTED_EDGE ( 'NONE', *, *, #170, .F. ) ;
#14910 = DIRECTION ( 'NONE',  ( -0.000000000000000000, -0.000000000000000000, -1.000000000000000000 ) ) ;
#14911 = DIRECTION ( 'NONE',  ( 0.000000000000000000, 0.000000000000000000, 1.000000000000000000 ) ) ;
#14912 =( LENGTH_UNIT ( ) NAMED_UNIT ( * ) SI_UNIT ( .MILLI., .METRE. ) );
#14913 = ORIENTED_EDGE ( 'NONE', *, *, #10093, .T. ) ;
#14914 = CARTESIAN_POINT ( 'NONE',  ( 1.039999999999996927, -25.12109765559644714, -12.52377138324250438 ) ) ;
#14915 = CIRCLE ( 'NONE', #8850, 4.500000000000000000 ) ;
#14916 = VERTEX_POINT ( 'NONE', #11855 ) ;
#14917 = FACE_OUTER_BOUND ( 'NONE', #8316, .T. ) ;
#14918 = CIRCLE ( 'NONE', #5651, 14.00000000000000178 ) ;
#14919 = CARTESIAN_POINT ( 'NONE',  ( 10.46874999795161720, 4.648860486681953397, -1.510506337161861667 ) ) ;
#14920 = EDGE_CURVE ( 'NONE', #312, #5246, #5155, .T. ) ;
#14921 = EDGE_CURVE ( 'NONE', #17528, #226, #11959, .T. ) ;
#14922 = CARTESIAN_POINT ( 'NONE',  ( 4.762500000000000178, 5.832380380939270108E-16, -6.502399999999998847 ) ) ;
#14923 = CARTESIAN_POINT ( 'NONE',  ( 16.19790265903627358, 9.644882309621939598, -32.00000000000000000 ) ) ;
#14924 = ORIENTED_EDGE ( 'NONE', *, *, #9837, .F. ) ;
#14925 = CARTESIAN_POINT ( 'NONE',  ( -0.5109457054262123155, -4.861323657744403448, -8.468749997951615427 ) ) ;
#14926 = CARTESIAN_POINT ( 'NONE',  ( 17.96448111170888851, 1.130229351527639148, -32.00000000000000000 ) ) ;
#14927 = ORIENTED_EDGE ( 'NONE', *, *, #17097, .T. ) ;
#14928 = VECTOR ( 'NONE', #4333, 1000.000000000000000 ) ;
#14929 = AXIS2_PLACEMENT_3D ( 'NONE', #5540, #10067, #19153 ) ;
#14930 = DIRECTION ( 'NONE',  ( -1.000000000000000000, -0.000000000000000000, -0.000000000000000000 ) ) ;
#14931 = CARTESIAN_POINT ( 'NONE',  ( -1.510506337161893642, -4.648860486681943627, -12.84374999795161543 ) ) ;
#14932 = ORIENTED_EDGE ( 'NONE', *, *, #7263, .T. ) ;
#14933 = FACE_OUTER_BOUND ( 'NONE', #5690, .T. ) ;
#14934 = CARTESIAN_POINT ( 'NONE',  ( -2.444050593749990341, 4.233219804643887585, -6.656249997951614539 ) ) ;
#14935 = CARTESIAN_POINT ( 'NONE',  ( 0.009102498987474663336, -21.10878525316950771, -12.54316204260915768 ) ) ;
#14936 = EDGE_LOOP ( 'NONE', ( #15121, #15173, #16369, #9675 ) ) ;
#14937 = CARTESIAN_POINT ( 'NONE',  ( 0.07181525696555274285, -24.78695292654917637, -5.344212458769628249 ) ) ;
#14938 = ORIENTED_EDGE ( 'NONE', *, *, #15321, .F. ) ;
#14939 = CARTESIAN_POINT ( 'NONE',  ( 0.7589665283900980386, -27.31260702007172725, -3.797536611356600034 ) ) ;
#14940 = EDGE_LOOP ( 'NONE', ( #2578, #10793 ) ) ;
#14941 = CARTESIAN_POINT ( 'NONE',  ( 11.58013454126452579, -14.56230589874905412, 35.00000000000000000 ) ) ;
#14942 = DIRECTION ( 'NONE',  ( -1.000000000000000000, -1.224646799147353207E-16, 0.000000000000000000 ) ) ;
#14943 = CARTESIAN_POINT ( 'NONE',  ( 2.246813503491803310, -4.409619785863921670, -9.968749997951617203 ) ) ;
#14944 = CARTESIAN_POINT ( 'NONE',  ( 13.46874999795161543, 0.5109457054262118714, -4.861323657744403448 ) ) ;
#14945 = VECTOR ( 'NONE', #3619, 1000.000000000000000 ) ;
#14946 = LINE ( 'NONE', #2631, #2159 ) ;
#14947 = VECTOR ( 'NONE', #8128, 1000.000000000000000 ) ;
#14948 = EDGE_LOOP ( 'NONE', ( #5991, #129, #30, #6570 ) ) ;
#14949 = DIRECTION ( 'NONE',  ( -0.000000000000000000, -0.000000000000000000, 1.000000000000000000 ) ) ;
#14950 = LINE ( 'NONE', #19155, #17423 ) ;
#14951 = ADVANCED_FACE ( 'NONE', ( #10662 ), #13355, .F. ) ;
#14952 = EDGE_CURVE ( 'NONE', #1526, #3180, #13876, .T. ) ;
#14953 = VERTEX_POINT ( 'NONE', #1552 ) ;
#14954 = DIRECTION ( 'NONE',  ( -0.8191520442889917986, 0.000000000000000000, -0.5735764363510460484 ) ) ;
#14955 = AXIS2_PLACEMENT_3D ( 'NONE', #7063, #15998, #893 ) ;
#14956 = DIRECTION ( 'NONE',  ( -1.000000000000000000, 0.000000000000000000, -0.000000000000000000 ) ) ;
#14957 = DIRECTION ( 'NONE',  ( 1.000000000000000000, 0.000000000000000000, 0.000000000000000000 ) ) ;
#14958 = CIRCLE ( 'NONE', #13039, 2.524999999999995470 ) ;
#14959 = EDGE_CURVE ( 'NONE', #17830, #4563, #7642, .T. ) ;
#14960 = DIRECTION ( 'NONE',  ( 0.000000000000000000, 0.000000000000000000, 1.000000000000000000 ) ) ;
#14961 = ORIENTED_EDGE ( 'NONE', *, *, #8389, .T. ) ;
#14962 = CARTESIAN_POINT ( 'NONE',  ( 1.988169868018593300, 4.465502636338023912, -9.468749997951615427 ) ) ;
#14963 =( LENGTH_UNIT ( ) NAMED_UNIT ( * ) SI_UNIT ( .MILLI., .METRE. ) );
#14964 = CARTESIAN_POINT ( 'NONE',  ( -4.861323657744403448, 0.5109457054262118714, -13.46874999795161543 ) ) ;
#14965 = DIRECTION ( 'NONE',  ( 1.000000000000000000, 0.000000000000000000, 0.000000000000000000 ) ) ;
#14966 = EDGE_LOOP ( 'NONE', ( #6431, #6331, #12423, #366 ) ) ;
#14967 = ORIENTED_EDGE ( 'NONE', *, *, #16066, .F. ) ;
#14968 = DIRECTION ( 'NONE',  ( 1.000000000000000000, 0.000000000000000000, 0.000000000000000000 ) ) ;
#14969 = EDGE_CURVE ( 'NONE', #17016, #2110, #13255, .T. ) ;
#14970 = CARTESIAN_POINT ( 'NONE',  ( -9.671566133830877376, 15.77352024078954429, -35.00000000000000000 ) ) ;
#14971 = EDGE_CURVE ( 'NONE', #15645, #4507, #5042, .T. ) ;
#14972 = ORIENTED_EDGE ( 'NONE', *, *, #11993, .T. ) ;
#14973 = ADVANCED_BREP_SHAPE_REPRESENTATION ( '', ( #3136, #16724 ), #8276 ) ;
#14974 = VECTOR ( 'NONE', #19073, 1000.000000000000000 ) ;
#14975 = DIRECTION ( 'NONE',  ( 0.000000000000000000, -1.000000000000000000, 0.000000000000000000 ) ) ;
#14976 = ORIENTED_EDGE ( 'NONE', *, *, #19711, .T. ) ;
#14977 = DIRECTION ( 'NONE',  ( -6.419766481290786633E-33, 1.000000000000000000, 0.000000000000000000 ) ) ;
#14978 = DIRECTION ( 'NONE',  ( 0.000000000000000000, 0.000000000000000000, 1.000000000000000000 ) ) ;
#14979 = ORIENTED_EDGE ( 'NONE', *, *, #19767, .T. ) ;
#14980 = ADVANCED_FACE ( 'NONE', ( #9658 ), #15655, .T. ) ;
#14981 = CARTESIAN_POINT ( 'NONE',  ( 2.789999999999999147, -7.909232158574988958, 24.34211360614297348 ) ) ;
#14982 = CARTESIAN_POINT ( 'NONE',  ( -2.620002426024580000, -5.142044285764733935, -13.81249999590322730 ) ) ;
#14983 = PRODUCT_DEFINITION_SHAPE ( 'NONE', 'NONE',  #2224 ) ;
#14984 = CIRCLE ( 'NONE', #933, 1.000000000000004441 ) ;
#14985 = ORIENTED_EDGE ( 'NONE', *, *, #9164, .F. ) ;
#14986 = CARTESIAN_POINT ( 'NONE',  ( 2.789999999999999147, 7.334849878007507762, 23.31896751603335005 ) ) ;
#14987 = ORIENTED_EDGE ( 'NONE', *, *, #408, .F. ) ;
#14988 = FACE_OUTER_BOUND ( 'NONE', #7283, .T. ) ;
#14989 = ADVANCED_FACE ( 'NONE', ( #12754 ), #7796, .T. ) ;
#14990 = FACE_BOUND ( 'NONE', #14339, .T. ) ;
#14991 = UNCERTAINTY_MEASURE_WITH_UNIT (LENGTH_MEASURE( 1.000000000000000082E-05 ), #10803, 'distance_accuracy_value', 'NONE');
#14992 = DIRECTION ( 'NONE',  ( -0.000000000000000000, -0.000000000000000000, 1.000000000000000000 ) ) ;
#14993 = PRODUCT_DEFINITION_FORMATION_WITH_SPECIFIED_SOURCE ( 'ANY', '', #15935, .NOT_KNOWN. ) ;
#14994 =( BOUNDED_CURVE ( )  B_SPLINE_CURVE ( 2, ( #13232, #17539, #1217, #5610, #6910, #19514, #16232 ),
 .UNSPECIFIED., .F., .F. ) 
 B_SPLINE_CURVE_WITH_KNOTS ( ( 3, 2, 2, 3 ),
 ( 0.1666819079834116757, 0.2000000000000000111, 0.2500000000000000000, 0.2843253191101273170 ),
 .UNSPECIFIED. ) 
 CURVE ( )  GEOMETRIC_REPRESENTATION_ITEM ( )  RATIONAL_B_SPLINE_CURVE ( ( 0.9945256517182512468, 0.9917959799814380917, 1.000000000000000000, 0.9876883405951377704, 1.000000000000000000, 0.9915479672430580482, 0.9947006833465674713 ) ) 
 REPRESENTATION_ITEM ( '' )  );
#14995 = CARTESIAN_POINT ( 'NONE',  ( 2.789999999999999147, -14.18181402625756959, 19.91106274590508107 ) ) ;
#14996 = CARTESIAN_POINT ( 'NONE',  ( 6.468749997951615427, 0.000000000000000000, -4.888101187500000222 ) ) ;
#14997 = VERTEX_POINT ( 'NONE', #10955 ) ;
#14998 = DIRECTION ( 'NONE',  ( 0.000000000000000000, 0.000000000000000000, 1.000000000000000000 ) ) ;
#14999 = CARTESIAN_POINT ( 'NONE',  ( -4.465502636338051445, -1.988169868018530462, -8.468749997951615427 ) ) ;
#15000 = CIRCLE ( 'NONE', #3166, 1.000000000000002665 ) ;
#15001 = VERTEX_POINT ( 'NONE', #10855 ) ;
#15002 = CARTESIAN_POINT ( 'NONE',  ( 14.81249999590322552, -5.574407415329169169, 1.493657965219485462 ) ) ;
#15003 = AXIS2_PLACEMENT_3D ( 'NONE', #9664, #5048, #6728 ) ;
#15004 = CARTESIAN_POINT ( 'NONE',  ( 0.02436607992776541887, 12.59161484032942901, -21.30679549418617924 ) ) ;
#15005 = CARTESIAN_POINT ( 'NONE',  ( 18.96448111170889206, 1.130229351527639148, 32.00000000000000000 ) ) ;
#15006 = CARTESIAN_POINT ( 'NONE',  ( -2.000000000000001776, 0.000000000000000000, 0.000000000000000000 ) ) ;
#15007 = EDGE_CURVE ( 'NONE', #6004, #6940, #18849, .T. ) ;
#15008 = ORIENTED_EDGE ( 'NONE', *, *, #18742, .F. ) ;
#15009 = CARTESIAN_POINT ( 'NONE',  ( 10.96874999795161720, 4.888101187500000222, -0.7741991708318890497 ) ) ;
#15010 = FILL_AREA_STYLE ('',( #8906 ) ) ;
#15011 = CARTESIAN_POINT ( 'NONE',  ( 1.999999999999998224, 0.000000000000000000, 0.000000000000000000 ) ) ;
#15012 = CARTESIAN_POINT ( 'NONE',  ( 13.50000000000000533, -4.080749450109621534, -4.080749450109677490 ) ) ;
#15013 = VERTEX_POINT ( 'NONE', #18649 ) ;
#15014 = CARTESIAN_POINT ( 'NONE',  ( 1.039999999999996261, 12.96210679857786197, 24.89775460606836788 ) ) ;
#15015 = VERTEX_POINT ( 'NONE', #6625 ) ;
#15016 = DIRECTION ( 'NONE',  ( 0.000000000000000000, 0.000000000000000000, -1.000000000000000000 ) ) ;
#15017 = ADVANCED_FACE ( 'NONE', ( #14150 ), #9461, .T. ) ;
#15018 = CARTESIAN_POINT ( 'NONE',  ( 1.749999999999998002, -12.52377138324206030, -25.12109765559667096 ) ) ;
#15019 = CARTESIAN_POINT ( 'NONE',  ( 2.031033465052724196, 27.14933624560908498, 4.828387785248115627 ) ) ;
#15020 = CARTESIAN_POINT ( 'NONE',  ( -1.773574444220725521, 4.620319390059830056, -7.343749997951615427 ) ) ;
#15021 = VECTOR ( 'NONE', #3716, 1000.000000000000000 ) ;
#15022 = ORIENTED_EDGE ( 'NONE', *, *, #7346, .T. ) ;
#15023 = CARTESIAN_POINT ( 'NONE',  ( 2.262072706628479590, 18.56460150496938155, 19.66369668717039332 ) ) ;
#15024 = B_SPLINE_CURVE_WITH_KNOTS ( 'NONE', 3,
 ( #10226, #2504, #5414, #11524, #19216, #16029 ),
 .UNSPECIFIED., .F., .F.,
 ( 4, 2, 4 ),
 ( 2.586195665736120714E-07, 0.001878649493629692274, 0.003757040367692811213 ),
 .UNSPECIFIED. ) ;
#15025 = DIRECTION ( 'NONE',  ( -0.000000000000000000, 0.000000000000000000, 1.000000000000000000 ) ) ;
#15026 = ORIENTED_EDGE ( 'NONE', *, *, #15427, .F. ) ;
#15027 = FACE_OUTER_BOUND ( 'NONE', #4404, .T. ) ;
#15028 = ADVANCED_FACE ( 'NONE', ( #3447, #6526 ), #12657, .T. ) ;
#15029 = CARTESIAN_POINT ( 'NONE',  ( -19.00000000000000355, 4.215373648918917304, 3.375000000000000888 ) ) ;
#15030 = ORIENTED_EDGE ( 'NONE', *, *, #12302, .T. ) ;
#15032 = CARTESIAN_POINT ( 'NONE',  ( 4.620319390059829168, 1.773574444220725299, -12.34374999795161543 ) ) ;
#15031 = CIRCLE ( 'NONE', #16304, 1.000000000000000000 ) ;
#15033 = DIRECTION ( 'NONE',  ( 1.000000000000000000, 0.000000000000000000, 0.000000000000000000 ) ) ;
#15034 = DIRECTION ( 'NONE',  ( -1.000000000000000000, -0.000000000000000000, -0.000000000000000000 ) ) ;
#15035 = EDGE_LOOP ( 'NONE', ( #10043, #1650 ) ) ;
#15036 = CARTESIAN_POINT ( 'NONE',  ( -2.000000000000001776, 0.000000000000000000, 4.400000000000000355 ) ) ;
#15037 = ORIENTED_EDGE ( 'NONE', *, *, #838, .F. ) ;
#15038 = CARTESIAN_POINT ( 'NONE',  ( 2.765633920072235519, 18.55949924794892780, 16.37294372382865504 ) ) ;
#15039 = VERTEX_POINT ( 'NONE', #17061 ) ;
#15040 = DIRECTION ( 'NONE',  ( -0.8660254037844383745, -0.5000000000000004441, 0.000000000000000000 ) ) ;
#15041 = ADVANCED_FACE ( 'NONE', ( #18747, #11153 ), #16961, .F. ) ;
#15042 = DIRECTION ( 'NONE',  ( 0.000000000000000000, 0.000000000000000000, -1.000000000000000000 ) ) ;
#15043 = CARTESIAN_POINT ( 'NONE',  ( -10.58013454126452224, -14.56230589874905235, -35.00000000000000000 ) ) ;
#15044 = CARTESIAN_POINT ( 'NONE',  ( -41.99999999999999289, -2.000000000000001776, 5.000000000000000000 ) ) ;
#15045 = CARTESIAN_POINT ( 'NONE',  ( 2.789999999999999147, -15.04425356660744839, -20.70663861606288236 ) ) ;
#15046 = ORIENTED_EDGE ( 'NONE', *, *, #19542, .T. ) ;
#15047 = DIRECTION ( 'NONE',  ( 0.000000000000000000, 0.000000000000000000, 1.000000000000000000 ) ) ;
#15048 = CONICAL_SURFACE ( 'NONE', #33, 4.000000000000000000, 0.2132412839022289897 ) ;
#15049 = CARTESIAN_POINT ( 'NONE',  ( 0.000000000000000000, 0.000000000000000000, -33.00000000000000000 ) ) ;
#15050 = EDGE_LOOP ( 'NONE', ( #3922, #15758 ) ) ;
#15051 = LINE ( 'NONE', #4445, #11856 ) ;
#15052 = EDGE_CURVE ( 'NONE', #16588, #479, #18523, .T. ) ;
#15053 = CARTESIAN_POINT ( 'NONE',  ( -9.000000000000001776, 1.102182119232617911E-15, 0.000000000000000000 ) ) ;
#15054 = PRODUCT_RELATED_PRODUCT_CATEGORY ( 'part', '', ( #19444 ) ) ;
#15055 = ORIENTED_EDGE ( 'NONE', *, *, #13411, .F. ) ;
#15056 = DIRECTION ( 'NONE',  ( 0.000000000000000000, 0.000000000000000000, 1.000000000000000000 ) ) ;
#15057 = CARTESIAN_POINT ( 'NONE',  ( 5.668774803599163192, 0.5958122406255991210, -9.000000000000005329 ) ) ;
#15058 = DIRECTION ( 'NONE',  ( -1.000000000000000000, -6.419766481290786633E-33, 0.000000000000000000 ) ) ;
#15059 = VERTEX_POINT ( 'NONE', #18452 ) ;
#15060 = FACE_OUTER_BOUND ( 'NONE', #7247, .T. ) ;
#15061 = DIRECTION ( 'NONE',  ( 0.000000000000000000, 0.000000000000000000, 1.000000000000000000 ) ) ;
#15062 = CIRCLE ( 'NONE', #2960, 28.06981291497571007 ) ;
#15063 = CARTESIAN_POINT ( 'NONE',  ( 5.668774803599156975, -0.5958122406256377568, -13.00000000000000533 ) ) ;
#15064 = CARTESIAN_POINT ( 'NONE',  ( -25.31088913245540084, -1.027644533213482535E-13, 41.99999999999999289 ) ) ;
#15065 = AXIS2_PLACEMENT_3D ( 'NONE', #8458, #16164, #4141 ) ;
#15066 = ORIENTED_EDGE ( 'NONE', *, *, #10242, .F. ) ;
#15067 = ORIENTED_EDGE ( 'NONE', *, *, #3459, .F. ) ;
#15068 = ADVANCED_FACE ( 'NONE', ( #246 ), #11249, .F. ) ;
#15069 = CARTESIAN_POINT ( 'NONE',  ( -1.869200000000000195, 0.000000000000000000, -6.760799999999997034 ) ) ;
#15070 = CARTESIAN_POINT ( 'NONE',  ( -2.068159791354184041, 5.387740456496233676, -7.812499995903224637 ) ) ;
#15071 = ORIENTED_EDGE ( 'NONE', *, *, #6224, .T. ) ;
#15072 = DIRECTION ( 'NONE',  ( 1.000000000000000000, 0.000000000000000000, 0.000000000000000000 ) ) ;
#15073 = ORIENTED_EDGE ( 'NONE', *, *, #13778, .F. ) ;
#15074 = CARTESIAN_POINT ( 'NONE',  ( 5.476417968967387750, 17.43449690031536292, 35.00000000000000000 ) ) ;
#15075 = EDGE_CURVE ( 'NONE', #7035, #11673, #5863, .T. ) ;
#15076 = CARTESIAN_POINT ( 'NONE',  ( 0.5279273620711166792, -12.96450951081199499, -23.73240184472509995 ) ) ;
#15077 = AXIS2_PLACEMENT_3D ( 'NONE', #3013, #15332, #2907 ) ;
#15078 = EDGE_LOOP ( 'NONE', ( #7210, #19446, #13707, #2232 ) ) ;
#15079 = AXIS2_PLACEMENT_3D ( 'NONE', #2679, #5681, #10404 ) ;
#15080 = AXIS2_PLACEMENT_3D ( 'NONE', #108, #10913, #12118 ) ;
#15081 = ADVANCED_FACE ( 'NONE', ( #4745 ), #2042, .F. ) ;
#15082 = CARTESIAN_POINT ( 'NONE',  ( 8.000000000000000000, 0.000000000000000000, 41.99999999999999289 ) ) ;
#15083 = CARTESIAN_POINT ( 'NONE',  ( 13.34374999795161365, 4.409619785863906571, 2.246813503491833508 ) ) ;
#15084 = CYLINDRICAL_SURFACE ( 'NONE', #17700, 9.000000000000021316 ) ;
#15085 = ORIENTED_EDGE ( 'NONE', *, *, #14792, .T. ) ;
#15086 = CARTESIAN_POINT ( 'NONE',  ( -18.96448111170889206, 1.130229351527647585, -32.00000000000000000 ) ) ;
#15087 = CYLINDRICAL_SURFACE ( 'NONE', #10306, 1.000000000000000888 ) ;
#15088 = ORIENTED_EDGE ( 'NONE', *, *, #10988, .F. ) ;
#15089 = FACE_OUTER_BOUND ( 'NONE', #1445, .T. ) ;
#15090 = AXIS2_PLACEMENT_3D ( 'NONE', #13601, #12106, #1983 ) ;
#15091 = FACE_BOUND ( 'NONE', #7975, .T. ) ;
#15092 = AXIS2_PLACEMENT_3D ( 'NONE', #15889, #14590, #6558 ) ;
#15093 = CARTESIAN_POINT ( 'NONE',  ( -5.700000000000001066, 1.090170143537592985E-15, -9.332722423957234170 ) ) ;
#15094 = VECTOR ( 'NONE', #10498, 1000.000000000000000 ) ;
#15095 = CARTESIAN_POINT ( 'NONE',  ( 17.11901729331276556, 5.562305898749055011, -32.00000000000000000 ) ) ;
#15096 = CARTESIAN_POINT ( 'NONE',  ( 0.02436607992776238310, -12.59161484032927092, 21.30679549418627161 ) ) ;
#15097 = EDGE_LOOP ( 'NONE', ( #10903, #9978, #17445, #5301 ) ) ;
#15098 = CARTESIAN_POINT ( 'NONE',  ( 1.394999999999999574, -25.12109765559644714, -12.52377138324250616 ) ) ;
#15099 = CIRCLE ( 'NONE', #14768, 6.200000000000021494 ) ;
#15100 = CARTESIAN_POINT ( 'NONE',  ( -4.620319390059805187, 1.773574444220789914, -10.96874999795161720 ) ) ;
#15101 = ORIENTED_EDGE ( 'NONE', *, *, #989, .T. ) ;
#15102 = CARTESIAN_POINT ( 'NONE',  ( 7.312499995903225525, 4.936344801571289409, 2.850000000000024070 ) ) ;
#15103 = CARTESIAN_POINT ( 'NONE',  ( 7.812499995903224637, -5.387740456496247887, 2.068159791354145849 ) ) ;
#15104 = CIRCLE ( 'NONE', #17022, 7.937500000000000000 ) ;
#15105 = AXIS2_PLACEMENT_3D ( 'NONE', #12442, #3335, #137 ) ;
#15106 = LINE ( 'NONE', #18209, #14774 ) ;
#15107 = CARTESIAN_POINT ( 'NONE',  ( 11.00000000000000711, 2.849999999999989431, 4.936344801571308061 ) ) ;
#15108 = VERTEX_POINT ( 'NONE', #18549 ) ;
#15109 = CLOSED_SHELL ( 'NONE', ( #900, #4482, #2337, #5231, #15881, #17284, #10770, #11895, #12533, #6950, #14063, #18027, #1380, #6710, #11654, #13769, #19456, #6466, #19248, #10912 ) ) ;
#15110 = DIRECTION ( 'NONE',  ( 0.000000000000000000, 0.000000000000000000, 1.000000000000000000 ) ) ;
#15111 = CYLINDRICAL_SURFACE ( 'NONE', #18990, 1.000000000000000888 ) ;
#15112 = TOROIDAL_SURFACE ( 'NONE', #1046, 24.12539914357697768, 8.000000000000000000 ) ;
#15113 = DIRECTION ( 'NONE',  ( 0.000000000000000000, 0.000000000000000000, -1.000000000000000000 ) ) ;
#15114 = ORIENTED_EDGE ( 'NONE', *, *, #5596, .T. ) ;
#15115 =( BOUNDED_SURFACE ( )  B_SPLINE_SURFACE ( 1, 2, ( 
 ( #10888, #14182, #16994, #278, #6556, #9289, #10985, #1877, #17186, #18680, #11082, #18778, #9586, #184, #8072, #6174, #3278 ),
 ( #5070, #16898, #7971, #11183, #373, #2072, #9695, #6455, #1779, #12295, #7870, #3179, #7778, #12588, #13891, #6267, #12487 ) ),
 .UNSPECIFIED., .F., .F., .F. ) 
 B_SPLINE_SURFACE_WITH_KNOTS ( ( 2, 2 ),
 ( 3, 2, 2, 2, 2, 2, 2, 2, 3 ),
 ( 0.000000000000000000, 1.000000000000000000 ),
 ( 0.000000000000000000, 0.05000000000000000278, 0.1000000000000000056, 0.1499999999999999944, 0.2000000000000000111, 0.2500000000000000000, 0.2999999999999999889, 0.3499999999999999778, 0.4000000000000000222 ),
 .UNSPECIFIED. ) 
 GEOMETRIC_REPRESENTATION_ITEM ( )  RATIONAL_B_SPLINE_SURFACE ( (
 ( 1.000000000000000000, 0.9876883405951377704, 1.000000000000000000, 0.9876883405951377704, 1.000000000000000000, 0.9876883405951377704, 1.000000000000000000, 0.9876883405951377704, 1.000000000000000000, 0.9876883405951377704, 1.000000000000000000, 0.9876883405951377704, 1.000000000000000000, 0.9876883405951377704, 1.000000000000000000, 0.9876883405951377704, 1.000000000000000000),
 ( 1.000000000000000000, 0.9876883405951377704, 1.000000000000000000, 0.9876883405951377704, 1.000000000000000000, 0.9876883405951377704, 1.000000000000000000, 0.9876883405951377704, 1.000000000000000000, 0.9876883405951377704, 1.000000000000000000, 0.9876883405951377704, 1.000000000000000000, 0.9876883405951377704, 1.000000000000000000, 0.9876883405951377704, 1.000000000000000000) ) ) 
 REPRESENTATION_ITEM ( '' )  SURFACE ( )  );
#15116 = DIRECTION ( 'NONE',  ( 0.000000000000000000, 0.000000000000000000, -1.000000000000000000 ) ) ;
#15117 = CARTESIAN_POINT ( 'NONE',  ( 7.468749997951615427, -1.510506337161893864, 4.648860486681943627 ) ) ;
#15118 = DIRECTION ( 'NONE',  ( -1.000000000000000000, -0.000000000000000000, -0.000000000000000000 ) ) ;
#15119 = CYLINDRICAL_SURFACE ( 'NONE', #1666, 0.9999999999999974465 ) ;
#15120 = FACE_OUTER_BOUND ( 'NONE', #18772, .T. ) ;
#15121 = ORIENTED_EDGE ( 'NONE', *, *, #17923, .F. ) ;
#15122 = CARTESIAN_POINT ( 'NONE',  ( -4.780397808154247308, 1.280903732194486722, -14.34374999795161365 ) ) ;
#15123 = CARTESIAN_POINT ( 'NONE',  ( 2.718184745196084773, 21.92234060054363809, -12.74223776959176568 ) ) ;
#15124 = ORIENTED_EDGE ( 'NONE', *, *, #13684, .F. ) ;
#15125 = AXIS2_PLACEMENT_3D ( 'NONE', #14833, #4225, #17735 ) ;
#15126 = AXIS2_PLACEMENT_3D ( 'NONE', #2858, #14747, #14845 ) ;
#15127 = ADVANCED_FACE ( 'NONE', ( #4844 ), #343, .F. ) ;
#15128 = DIRECTION ( 'NONE',  ( 0.000000000000000000, -1.000000000000000000, 0.000000000000000000 ) ) ;
#15129 = CARTESIAN_POINT ( 'NONE',  ( -5.209999999999999964, 0.000000000000000000, 0.000000000000000000 ) ) ;
#15130 = ORIENTED_EDGE ( 'NONE', *, *, #12842, .T. ) ;
#15131 = CARTESIAN_POINT ( 'NONE',  ( 1.988169868018593300, 4.465502636338023912, -9.843749997951615427 ) ) ;
#15132 = DIRECTION ( 'NONE',  ( -1.000000000000000000, 0.000000000000000000, 0.000000000000000000 ) ) ;
#15133 = CARTESIAN_POINT ( 'NONE',  ( -5.209999999999999964, 0.000000000000000000, 0.000000000000000000 ) ) ;
#15134 = ORIENTED_EDGE ( 'NONE', *, *, #19296, .T. ) ;
#15135 = CARTESIAN_POINT ( 'NONE',  ( 0.000000000000000000, 0.000000000000000000, -30.00000000000000355 ) ) ;
#15136 = ORIENTED_EDGE ( 'NONE', *, *, #10006, .F. ) ;
#15137 = CARTESIAN_POINT ( 'NONE',  ( 5.500000000000005329, 0.000000000000000000, 0.000000000000000000 ) ) ;
#15138 = VERTEX_POINT ( 'NONE', #11736 ) ;
#15139 = CARTESIAN_POINT ( 'NONE',  ( 2.789999999999999147, 25.59481291497571220, 0.000000000000000000 ) ) ;
#15140 = AXIS2_PLACEMENT_3D ( 'NONE', #1200, #12107, #7685 ) ;
#15141 = CARTESIAN_POINT ( 'NONE',  ( 0.000000000000000000, -12.52067188844335988, -20.62201879784928238 ) ) ;
#15142 = CARTESIAN_POINT ( 'NONE',  ( 0.000000000000000000, 0.000000000000000000, -6.000000000000005329 ) ) ;
#15143 = CARTESIAN_POINT ( 'NONE',  ( 6.500000000000005329, -5.387740456496247887, 2.068159791354145849 ) ) ;
#15144 = CARTESIAN_POINT ( 'NONE',  ( 13.00000000000000178, 0.6516788101670740740, 4.844895625238696546 ) ) ;
#15145 = ORIENTED_EDGE ( 'NONE', *, *, #10201, .F. ) ;
#15146 = CARTESIAN_POINT ( 'NONE',  ( 13.00000000000000533, -4.859449410165145977, 2.460251518383743896 ) ) ;
#15147 = AXIS2_PLACEMENT_3D ( 'NONE', #8540, #18845, #14449 ) ;
#15148 = CARTESIAN_POINT ( 'NONE',  ( -5.626241948324210540, -16.73597674598852336, 32.00000000000000000 ) ) ;
#15149 = ORIENTED_EDGE ( 'NONE', *, *, #9471, .F. ) ;
#15150 = EDGE_CURVE ( 'NONE', #4430, #11599, #15803, .T. ) ;
#15151 = CIRCLE ( 'NONE', #13243, 0.1999999999999996503 ) ;
#15152 = CARTESIAN_POINT ( 'NONE',  ( 0.000000000000000000, 15.04425356660760293, 20.70663861606276868 ) ) ;
#15153 = CARTESIAN_POINT ( 'NONE',  ( 8.000000000000000000, 1.999999999999997335, 37.99999999999999289 ) ) ;
#15154 = ORIENTED_EDGE ( 'NONE', *, *, #2547, .F. ) ;
#15155 = CARTESIAN_POINT ( 'NONE',  ( 0.000000000000000000, 0.000000000000000000, 35.00000000000000000 ) ) ;
#15156 = DIRECTION ( 'NONE',  ( 1.000000000000000000, 0.000000000000000000, 0.000000000000000000 ) ) ;
#15157 = DIRECTION ( 'NONE',  ( -1.000000000000000000, 0.000000000000000000, -0.000000000000000000 ) ) ;
#15158 = ORIENTED_EDGE ( 'NONE', *, *, #16534, .F. ) ;
#15159 = DIRECTION ( 'NONE',  ( 1.000000000000000000, 0.000000000000000000, 0.000000000000000000 ) ) ;
#15160 = VECTOR ( 'NONE', #16685, 1000.000000000000000 ) ;
#15161 = DIRECTION ( 'NONE',  ( 8.326672684688675286E-17, -3.014080362966024110E-31, -1.000000000000000000 ) ) ;
#15162 = CARTESIAN_POINT ( 'NONE',  ( 2.030753602223783094, -4.828194074574165384, -27.14986936243579763 ) ) ;
#15163 = CARTESIAN_POINT ( 'NONE',  ( 0.3020334839682081163, -5.763142191869158992, -8.812499995903225525 ) ) ;
#15164 = ORIENTED_EDGE ( 'NONE', *, *, #14366, .T. ) ;
#15165 = ORIENTED_EDGE ( 'NONE', *, *, #17755, .T. ) ;
#15166 = CARTESIAN_POINT ( 'NONE',  ( -2.444050593750049849, -4.233219804643852946, -6.468749997951615427 ) ) ;
#15167 = CARTESIAN_POINT ( 'NONE',  ( 4.484949146646379781, 3.631840208645794821, -11.81249999590322552 ) ) ;
#15169 = ORIENTED_EDGE ( 'NONE', *, *, #4390, .F. ) ;
#15168 = VECTOR ( 'NONE', #9531, 1000.000000000000000 ) ;
#15170 = ADVANCED_FACE ( 'NONE', ( #14743 ), #5240, .F. ) ;
#15171 = EDGE_CURVE ( 'NONE', #283, #6839, #10420, .T. ) ;
#15172 = CARTESIAN_POINT ( 'NONE',  ( 2.789999999999999147, 15.04425356660790136, -20.70663861606255196 ) ) ;
#15173 = ORIENTED_EDGE ( 'NONE', *, *, #18823, .T. ) ;
#15174 = CARTESIAN_POINT ( 'NONE',  ( 1.800000000000000044, 0.000000000000000000, -7.800000000000000711 ) ) ;
#15175 = EDGE_CURVE ( 'NONE', #19072, #17360, #16157, .T. ) ;
#15176 = VECTOR ( 'NONE', #7031, 1000.000000000000000 ) ;
#15177 = ORIENTED_EDGE ( 'NONE', *, *, #5206, .F. ) ;
#15178 = EDGE_CURVE ( 'NONE', #155, #3939, #11960, .T. ) ;
#15179 = CARTESIAN_POINT ( 'NONE',  ( 0.000000000000000000, 0.000000000000000000, 0.000000000000000000 ) ) ;
#15180 = CARTESIAN_POINT ( 'NONE',  ( 14.31249999590322552, 4.611396867937201272, 3.350375938067096548 ) ) ;
#15181 = CARTESIAN_POINT ( 'NONE',  ( -3.350375938067128967, -4.611396867937178179, -14.31249999590322552 ) ) ;
#15182 = ORIENTED_EDGE ( 'NONE', *, *, #9030, .T. ) ;
#15183 = DIRECTION ( 'NONE',  ( 1.000000000000000000, 0.000000000000000000, 0.000000000000000000 ) ) ;
#15184 = DIRECTION ( 'NONE',  ( -1.000000000000000000, 0.000000000000000000, 0.000000000000000000 ) ) ;
#15185 = ORIENTED_EDGE ( 'NONE', *, *, #6477, .F. ) ;
#15186 = EDGE_CURVE ( 'NONE', #18537, #4447, #17742, .T. ) ;
#15187 = CARTESIAN_POINT ( 'NONE',  ( 2.765633920072235963, -5.391175441198450713, -24.15498966839968276 ) ) ;
#15188 = CIRCLE ( 'NONE', #8802, 3.797000000000000597 ) ;
#15189 = CARTESIAN_POINT ( 'NONE',  ( 2.789999999999999147, 7.334849878007844382, -23.31896751603323992 ) ) ;
#15190 = CIRCLE ( 'NONE', #7471, 24.12539914357697413 ) ;
#15191 = LINE ( 'NONE', #13483, #6384 ) ;
#15192 = CARTESIAN_POINT ( 'NONE',  ( 0.02436607992775978102, 24.63872515616082737, 2.336989772644355146 ) ) ;
#15193 = PRODUCT_RELATED_PRODUCT_CATEGORY ( 'part', '', ( #5221 ) ) ;
#15194 = CARTESIAN_POINT ( 'NONE',  ( 2.000000000000001776, 0.000000000000000000, 0.000000000000000000 ) ) ;
#15195 = ADVANCED_FACE ( 'NONE', ( #1031 ), #8453, .F. ) ;
#15196 = ORIENTED_EDGE ( 'NONE', *, *, #19203, .T. ) ;
#15197 = DIRECTION ( 'NONE',  ( 0.000000000000000000, 0.000000000000000000, -1.000000000000000000 ) ) ;
#15198 = CARTESIAN_POINT ( 'NONE',  ( -0.5109457054261112852, 4.861323657744413218, -14.46874999795161720 ) ) ;
#15199 = APPLICATION_CONTEXT ( 'automotive_design' ) ;
#15200 = EDGE_LOOP ( 'NONE', ( #19053, #1938 ) ) ;
#15201 = B_SPLINE_CURVE_WITH_KNOTS ( 'NONE', 3,
 ( #16709, #12200, #1199, #7482, #1592, #11903 ),
 .UNSPECIFIED., .F., .F.,
 ( 4, 2, 4 ),
 ( 2.132675795045763710E-07, 0.001878604073277002169, 0.003756994878974500001 ),
 .UNSPECIFIED. ) ;
#15202 = CARTESIAN_POINT ( 'NONE',  ( 8.812499995903225525, 3.143139765844590983, 4.840010801796506890 ) ) ;
#15203 = EDGE_CURVE ( 'NONE', #3148, #6388, #9752, .T. ) ;
#15204 = EDGE_CURVE ( 'NONE', #5957, #4210, #5878, .T. ) ;
#15205 = CARTESIAN_POINT ( 'NONE',  ( 13.31249999590322730, -1.185096637661177343, -5.575441324182703440 ) ) ;
#15206 = AXIS2_PLACEMENT_3D ( 'NONE', #12762, #14362, #2250 ) ;
#15207 = AXIS2_PLACEMENT_3D ( 'NONE', #15644, #1928, #5227 ) ;
#15208 = LINE ( 'NONE', #15005, #5494 ) ;
#15209 = CARTESIAN_POINT ( 'NONE',  ( 7.500000000000005329, 5.763142191869157216, -0.3020334839682475847 ) ) ;
#15210 = ORIENTED_EDGE ( 'NONE', *, *, #15222, .T. ) ;
#15211 = CARTESIAN_POINT ( 'NONE',  ( 6.468749997951615427, 0.000000000000000000, -4.888101187500000222 ) ) ;
#15212 = CARTESIAN_POINT ( 'NONE',  ( 3.270778111535314281, -3.632567103900546712, -12.84374999795161543 ) ) ;
#15213 = ADVANCED_FACE ( 'NONE', ( #17456 ), #6926, .T. ) ;
#15214 = DIRECTION ( 'NONE',  ( 1.000000000000000000, -0.000000000000000000, -0.000000000000000000 ) ) ;
#15215 = EDGE_LOOP ( 'NONE', ( #3411, #12780 ) ) ;
#15216 = CARTESIAN_POINT ( 'NONE',  ( -12.86923836996420611, -11.47363181547641275, -32.00000000000000000 ) ) ;
#15217 = CARTESIAN_POINT ( 'NONE',  ( 13.84374999795161543, -4.465502636338038123, 1.988169868018562880 ) ) ;
#15218 = CARTESIAN_POINT ( 'NONE',  ( 12.73273607671833929, -4.522548057701222923, -1.899256020376466569 ) ) ;
#15219 = CARTESIAN_POINT ( 'NONE',  ( 10.96874999795161720, 4.888101187500000222, -0.7741991708318890497 ) ) ;
#15220 = ORIENTED_EDGE ( 'NONE', *, *, #13519, .T. ) ;
#15221 = CARTESIAN_POINT ( 'NONE',  ( 2.789999999999999147, 15.74360496233408213, -18.28042085475260592 ) ) ;
#15222 = EDGE_CURVE ( 'NONE', #18023, #11483, #3000, .T. ) ;
#15223 = AXIS2_PLACEMENT_3D ( 'NONE', #14740, #17835, #10143 ) ;
#15224 = CARTESIAN_POINT ( 'NONE',  ( 4.620319390059829168, 1.773574444220725743, -12.34374999795161543 ) ) ;
#15225 = EDGE_CURVE ( 'NONE', #2419, #17102, #12294, .T. ) ;
#15226 = AXIS2_PLACEMENT_3D ( 'NONE', #2608, #3925, #19222 ) ;
#15227 = ORIENTED_EDGE ( 'NONE', *, *, #3106, .T. ) ;
#15228 = DIRECTION ( 'NONE',  ( -1.000000000000000000, -0.000000000000000000, 0.000000000000000000 ) ) ;
#15229 = FACE_OUTER_BOUND ( 'NONE', #18253, .T. ) ;
#15230 = ORIENTED_EDGE ( 'NONE', *, *, #18090, .T. ) ;
#15231 = CARTESIAN_POINT ( 'NONE',  ( -4.648860486681953397, 1.510506337161861445, -7.468749997951615427 ) ) ;
#15232 = LINE ( 'NONE', #13, #17043 ) ;
#15233 =( BOUNDED_CURVE ( )  B_SPLINE_CURVE ( 2, ( #3151, #11963, #7438, #15163, #16471, #50, #7749, #16667, #2948, #18267, #15367, #4552, #3049, #154, #1654 ),
 .UNSPECIFIED., .F., .F. ) 
 B_SPLINE_CURVE_WITH_KNOTS ( ( 3, 2, 2, 2, 2, 2, 2, 3 ),
 ( 0.000000000000000000, 0.05000000000000000278, 0.1000000000000000056, 0.1499999999999999944, 0.2000000000000000111, 0.2500000000000000000, 0.2999999999999999889, 0.3333180920165860761 ),
 .UNSPECIFIED. ) 
 CURVE ( )  GEOMETRIC_REPRESENTATION_ITEM ( )  RATIONAL_B_SPLINE_CURVE ( ( 1.000000000000000000, 0.9876883405951377704, 1.000000000000000000, 0.9876883405951377704, 1.000000000000000000, 0.9876883405951377704, 1.000000000000000000, 0.9876883405951377704, 1.000000000000000000, 0.9876883405951377704, 1.000000000000000000, 0.9876883405951377704, 1.000000000000000000, 0.9917959799814386468, 0.9945256517182510247 ) ) 
 REPRESENTATION_ITEM ( '' )  );
#15234 = ORIENTED_EDGE ( 'NONE', *, *, #11409, .T. ) ;
#15235 = AXIS2_PLACEMENT_3D ( 'NONE', #10217, #2994, #16713 ) ;
#15236 = CARTESIAN_POINT ( 'NONE',  ( 8.312499995903225525, 5.575441324182696334, -1.185096637661215535 ) ) ;
#15237 = CARTESIAN_POINT ( 'NONE',  ( -2.246813503491833508, 4.409619785863906571, -9.968749997951615427 ) ) ;
#15238 = VECTOR ( 'NONE', #6272, 1000.000000000000114 ) ;
#15239 = ADVANCED_FACE ( 'NONE', ( #651 ), #940, .F. ) ;
#15240 = ORIENTED_EDGE ( 'NONE', *, *, #3708, .F. ) ;
#15241 = DIRECTION ( 'NONE',  ( 0.000000000000000000, 0.000000000000000000, -1.000000000000000000 ) ) ;
#15242 = ORIENTED_EDGE ( 'NONE', *, *, #16786, .T. ) ;
#15243 = CARTESIAN_POINT ( 'NONE',  ( -7.937500000000000000, 4.582717761692651770, -6.527800000000000047 ) ) ;
#15244 = ORIENTED_EDGE ( 'NONE', *, *, #4982, .F. ) ;
#15245 = CARTESIAN_POINT ( 'NONE',  ( 17.28688694438834972, -7.664027248171309203, 32.00000000000000000 ) ) ;
#15246 = DIRECTION ( 'NONE',  ( 0.000000000000000000, 0.000000000000000000, 1.000000000000000000 ) ) ;
#15247 = FACE_BOUND ( 'NONE', #4956, .T. ) ;
#15248 = CARTESIAN_POINT ( 'NONE',  ( -0.000000000000000000, 0.000000000000000000, 0.000000000000000000 ) ) ;
#15249 = EDGE_CURVE ( 'NONE', #17369, #6321, #19331, .T. ) ;
#15250 = CARTESIAN_POINT ( 'NONE',  ( 0.5279273381794633568, -3.461047254864449307, 26.82026385750176445 ) ) ;
#15251 = EDGE_CURVE ( 'NONE', #15528, #10889, #7266, .T. ) ;
#15252 = VERTEX_POINT ( 'NONE', #9865 ) ;
#15253 = B_SPLINE_CURVE_WITH_KNOTS ( 'NONE', 3,
 ( #19509, #16525, #2803, #5798 ),
 .UNSPECIFIED., .F., .F.,
 ( 4, 4 ),
 ( 0.000000000000000000, 0.001125480700308659470 ),
 .UNSPECIFIED. ) ;
#15254 = CARTESIAN_POINT ( 'NONE',  ( 2.789999999999999147, -5.456805104201270851, 23.69843731927166885 ) ) ;
#15255 = AXIS2_PLACEMENT_3D ( 'NONE', #16793, #7958, #10779 ) ;
#15256 = VECTOR ( 'NONE', #2025, 1000.000000000000000 ) ;
#15257 = ORIENTED_EDGE ( 'NONE', *, *, #3095, .F. ) ;
#15258 = EDGE_CURVE ( 'NONE', #8477, #11999, #8746, .T. ) ;
#15259 = CARTESIAN_POINT ( 'NONE',  ( 2.783068961317272549, 21.08061549536614976, 12.53626894672835945 ) ) ;
#15260 = CARTESIAN_POINT ( 'NONE',  ( 2.789999999999999147, -22.25075486061731667, -9.324097380959683434 ) ) ;
#15261 = ORIENTED_EDGE ( 'NONE', *, *, #3929, .F. ) ;
#15262 = CARTESIAN_POINT ( 'NONE',  ( -17.68117051311639898, -3.372863662543042818, -32.00000000000000000 ) ) ;
#15263 = CARTESIAN_POINT ( 'NONE',  ( 3.270778111535314281, -3.632567103900546712, -12.46874999795161543 ) ) ;
#15264 = ORIENTED_EDGE ( 'NONE', *, *, #1055, .T. ) ;
#15265 = CARTESIAN_POINT ( 'NONE',  ( 4.781284448697194378, 1.016293382781411792, -12.46874999795161543 ) ) ;
#15266 = CIRCLE ( 'NONE', #16551, 1.000000000000004441 ) ;
#15267 = CARTESIAN_POINT ( 'NONE',  ( 0.000000000000000000, 0.000000000000000000, 0.000000000000000000 ) ) ;
#15268 = CARTESIAN_POINT ( 'NONE',  ( -2.068159791354183596, 5.387740456496233676, -6.500000000000005329 ) ) ;
#15269 = VECTOR ( 'NONE', #19737, 1000.000000000000000 ) ;
#15270 = CARTESIAN_POINT ( 'NONE',  ( -2.255998204157477538, -17.85806462366060288, -32.00000000000000000 ) ) ;
#15271 = EDGE_LOOP ( 'NONE', ( #12411, #4392, #6662, #11874 ) ) ;
#15272 = ORIENTED_EDGE ( 'NONE', *, *, #2245, .F. ) ;
#15273 = DIRECTION ( 'NONE',  ( 1.000000000000000000, 0.000000000000000000, 0.000000000000000000 ) ) ;
#15274 = CARTESIAN_POINT ( 'NONE',  ( 3.270778111535338262, 3.632567103900524064, -10.84374999795161543 ) ) ;
#15275 = ADVANCED_FACE ( 'NONE', ( #1327 ), #9032, .T. ) ;
#15276 = ORIENTED_EDGE ( 'NONE', *, *, #19666, .T. ) ;
#15277 = DIRECTION ( 'NONE',  ( 0.000000000000000000, 0.000000000000000000, 1.000000000000000000 ) ) ;
#15278 = ORIENTED_EDGE ( 'NONE', *, *, #14385, .T. ) ;
#15279 = FILL_AREA_STYLE_COLOUR ( '', #10951 ) ;
#15280 = VECTOR ( 'NONE', #10196, 1000.000000000000000 ) ;
#15281 = ORIENTED_EDGE ( 'NONE', *, *, #9903, .T. ) ;
#15282 = EDGE_CURVE ( 'NONE', #2041, #9230, #9927, .T. ) ;
#15283 = DIRECTION ( 'NONE',  ( 1.000000000000000000, 1.224646799147353207E-16, 0.000000000000000000 ) ) ;
#15284 = DIRECTION ( 'NONE',  ( -1.000000000000000000, 0.000000000000000000, 0.000000000000000000 ) ) ;
#15285 = EDGE_CURVE ( 'NONE', #6248, #3602, #1530, .T. ) ;
#15286 = CYLINDRICAL_SURFACE ( 'NONE', #9079, 12.00000000000000178 ) ;
#15287 = EDGE_LOOP ( 'NONE', ( #2795, #2949 ) ) ;
#15288 = VERTEX_POINT ( 'NONE', #5917 ) ;
#15289 = CARTESIAN_POINT ( 'NONE',  ( 1.039999999999996483, -19.67366047555544384, 20.02152543075338897 ) ) ;
#15290 = CARTESIAN_POINT ( 'NONE',  ( 13.86923836996420789, -11.47363181547641453, -35.00000000000000000 ) ) ;
#15291 = ORIENTED_EDGE ( 'NONE', *, *, #6616, .F. ) ;
#15292 = CARTESIAN_POINT ( 'NONE',  ( 2.789999999999999591, 12.51294990530046292, -20.85230829256839513 ) ) ;
#15293 = CIRCLE ( 'NONE', #1547, 8.265000000000021885 ) ;
#15294 = FACE_BOUND ( 'NONE', #15616, .T. ) ;
#15295 = CARTESIAN_POINT ( 'NONE',  ( 0.02436607992776411782, -24.63872515616084513, 2.336989772644183283 ) ) ;
#15296 = EDGE_CURVE ( 'NONE', #4507, #8343, #4474, .T. ) ;
#15297 = ADVANCED_FACE ( 'NONE', ( #11834 ), #13531, .F. ) ;
#15298 = DIRECTION ( 'NONE',  ( 0.000000000000000000, 0.000000000000000000, 1.000000000000000000 ) ) ;
#15299 = CARTESIAN_POINT ( 'NONE',  ( 2.246813503491833508, 4.409619785863906571, -13.34374999795161365 ) ) ;
#15300 = ORIENTED_EDGE ( 'NONE', *, *, #2266, .F. ) ;
#15301 = CARTESIAN_POINT ( 'NONE',  ( 2.262072625383134916, -26.57710921259758408, -4.996265754456650221 ) ) ;
#15302 = CARTESIAN_POINT ( 'NONE',  ( 0.000000000000000000, 0.000000000000000000, 0.000000000000000000 ) ) ;
#15303 = VERTEX_POINT ( 'NONE', #12039 ) ;
#15304 = CARTESIAN_POINT ( 'NONE',  ( 0.000000000000000000, -1.991882183130148087, -24.04302995059968140 ) ) ;
#15305 = B_SPLINE_CURVE_WITH_KNOTS ( 'NONE', 3,
 ( #18803, #7519, #19735, #16748 ),
 .UNSPECIFIED., .F., .F.,
 ( 4, 4 ),
 ( 0.005258105385878709091, 0.005948373736081389272 ),
 .UNSPECIFIED. ) ;
#15306 = CARTESIAN_POINT ( 'NONE',  ( 9.312499995903225525, -5.668774803599153422, -0.5958122406256771697 ) ) ;
#15307 = VECTOR ( 'NONE', #6836, 1000.000000000000000 ) ;
#15308 = LINE ( 'NONE', #8902, #18595 ) ;
#15309 = DIRECTION ( 'NONE',  ( 0.000000000000000000, 0.000000000000000000, -1.000000000000000000 ) ) ;
#15310 = ORIENTED_EDGE ( 'NONE', *, *, #2097, .F. ) ;
#15311 = DIRECTION ( 'NONE',  ( 1.000000000000000000, 0.000000000000000000, 0.000000000000000000 ) ) ;
#15312 =( NAMED_UNIT ( * ) SI_UNIT ( $, .STERADIAN. ) SOLID_ANGLE_UNIT ( ) );
#15313 = CARTESIAN_POINT ( 'NONE',  ( -16.28688694438836038, -7.664027248171298545, 32.00000000000000000 ) ) ;
#15314 = EDGE_LOOP ( 'NONE', ( #14031, #188 ) ) ;
#15315 = DIRECTION ( 'NONE',  ( 1.000000000000000000, 0.000000000000000000, 0.000000000000000000 ) ) ;
#15316 = CARTESIAN_POINT ( 'NONE',  ( 10.46874999795161720, -1.016293382781444654, 4.781284448697187273 ) ) ;
#15317 = DIRECTION ( 'NONE',  ( -0.000000000000000000, -0.000000000000000000, 1.000000000000000000 ) ) ;
#15318 = EDGE_CURVE ( 'NONE', #9982, #9207, #18140, .T. ) ;
#15319 = DIRECTION ( 'NONE',  ( -0.9340060080012921873, 0.000000000000000000, 0.3572572980605013271 ) ) ;
#15320 = ORIENTED_EDGE ( 'NONE', *, *, #7278, .T. ) ;
#15321 = EDGE_CURVE ( 'NONE', #18731, #1773, #16636, .T. ) ;
#15322 = DIRECTION ( 'NONE',  ( -1.000000000000000000, 0.000000000000000000, 0.000000000000000000 ) ) ;
#15323 = AXIS2_PLACEMENT_3D ( 'NONE', #18355, #17153, #12556 ) ;
#15324 = LINE ( 'NONE', #3107, #5355 ) ;
#15325 = ORIENTED_EDGE ( 'NONE', *, *, #14313, .F. ) ;
#15326 = CARTESIAN_POINT ( 'NONE',  ( 9.468749997951615427, -3.954556930911881985, 2.873153789725797491 ) ) ;
#15327 = DIRECTION ( 'NONE',  ( 0.000000000000000000, 0.000000000000000000, 1.000000000000000000 ) ) ;
#15328 = AXIS2_PLACEMENT_3D ( 'NONE', #2343, #851, #5438 ) ;
#15329 = ORIENTED_EDGE ( 'NONE', *, *, #11247, .F. ) ;
#15330 = CARTESIAN_POINT ( 'NONE',  ( 12.50000000000000533, 4.840010801796527318, -3.143139765844555900 ) ) ;
#15331 = EDGE_CURVE ( 'NONE', #9218, #283, #11934, .T. ) ;
#15332 = DIRECTION ( 'NONE',  ( -0.000000000000000000, -0.000000000000000000, 1.000000000000000000 ) ) ;
#15333 = CARTESIAN_POINT ( 'NONE',  ( -15.00000000000000355, -4.215373648918918192, 3.375000000000000888 ) ) ;
#15334 = ORIENTED_EDGE ( 'NONE', *, *, #2734, .T. ) ;
#15335 = DIRECTION ( 'NONE',  ( 0.000000000000000000, -0.5877852522924684742, -0.8090169943749507819 ) ) ;
#15337 = ADVANCED_FACE ( 'NONE', ( #19729, #6014 ), #10247, .T. ) ;
#15336 = ADVANCED_FACE ( 'NONE', ( #16741 ), #19525, .T. ) ;
#15338 = FACE_BOUND ( 'NONE', #10825, .T. ) ;
#15339 = ORIENTED_EDGE ( 'NONE', *, *, #10407, .T. ) ;
#15340 = CARTESIAN_POINT ( 'NONE',  ( 0.02436607992776325046, 16.37294372382858398, 18.55949924794898465 ) ) ;
#15341 = EDGE_LOOP ( 'NONE', ( #18056, #9532, #12152, #9302 ) ) ;
#15342 = PLANE ( 'NONE',  #1816 ) ;
#15343 = ORIENTED_EDGE ( 'NONE', *, *, #259, .F. ) ;
#15344 = AXIS2_PLACEMENT_3D ( 'NONE', #19310, #13123, #5601 ) ;
#15345 = B_SPLINE_CURVE_WITH_KNOTS ( 'NONE', 3,
 ( #10669, #9468, #3052, #12569, #7847, #4957 ),
 .UNSPECIFIED., .F., .F.,
 ( 4, 2, 4 ),
 ( 1.979325885420462316E-07, 0.001878588715165608420, 0.003756979497742674902 ),
 .UNSPECIFIED. ) ;
#15346 = PRESENTATION_STYLE_ASSIGNMENT (( #12142 ) ) ;
#15347 = CARTESIAN_POINT ( 'NONE',  ( 2.765633920072242624, -22.71065055754459650, 9.836394144775621129 ) ) ;
#15348 = CARTESIAN_POINT ( 'NONE',  ( 8.000000000000000000, 0.000000000000000000, 0.000000000000000000 ) ) ;
#15349 = CARTESIAN_POINT ( 'NONE',  ( 10.46874999795161720, 3.632567103900523620, 3.270778111535338262 ) ) ;
#15350 = ORIENTED_EDGE ( 'NONE', *, *, #15052, .T. ) ;
#15351 = CARTESIAN_POINT ( 'NONE',  ( 5.021782490506621954, -2.235841616153703360, -14.11718749948790830 ) ) ;
#15352 = DIRECTION ( 'NONE',  ( 0.000000000000000000, 0.000000000000000000, 1.000000000000000000 ) ) ;
#15353 = CIRCLE ( 'NONE', #6705, 0.03079999999999923077 ) ;
#15354 = VERTEX_POINT ( 'NONE', #21 ) ;
#15355 = AXIS2_PLACEMENT_3D ( 'NONE', #14429, #6994, #5214 ) ;
#15356 = B_SPLINE_CURVE_WITH_KNOTS ( 'NONE', 3,
 ( #13733, #12239, #10734, #1626 ),
 .UNSPECIFIED., .F., .F.,
 ( 4, 4 ),
 ( 2.135345996173300665E-07, 0.0006888010880210822381 ),
 .UNSPECIFIED. ) ;
#15357 = CARTESIAN_POINT ( 'NONE',  ( 2.765633920072239516, 21.30679549418631780, 12.59161484032919986 ) ) ;
#15358 = FACE_OUTER_BOUND ( 'NONE', #6418, .T. ) ;
#15359 = ORIENTED_EDGE ( 'NONE', *, *, #4793, .F. ) ;
#15360 = CARTESIAN_POINT ( 'NONE',  ( 12.00000000000000533, -1.185096637661177343, -5.575441324182703440 ) ) ;
#15361 = SURFACE_SIDE_STYLE ('',( #3043 ) ) ;
#15362 = ORIENTED_EDGE ( 'NONE', *, *, #1733, .F. ) ;
#15363 = DIRECTION ( 'NONE',  ( 1.000000000000000000, 0.000000000000000000, 0.000000000000000000 ) ) ;
#15364 = ORIENTED_EDGE ( 'NONE', *, *, #2441, .T. ) ;
#15365 = PRODUCT_CONTEXT ( 'NONE', #12515, 'mechanical' ) ;
#15366 = CARTESIAN_POINT ( 'NONE',  ( 2.262072637928881580, 12.96450951081251191, -23.73240184472483350 ) ) ;
#15367 = CARTESIAN_POINT ( 'NONE',  ( -4.936344801571327601, -2.849999999999954792, -12.31249999590322552 ) ) ;
#15368 = ORIENTED_EDGE ( 'NONE', *, *, #12019, .T. ) ;
#15369 = VERTEX_POINT ( 'NONE', #13428 ) ;
#15370 = CARTESIAN_POINT ( 'NONE',  ( 0.006931038682726457442, 12.53626894672828485, 21.08061549536619950 ) ) ;
#15371 = AXIS2_PLACEMENT_3D ( 'NONE', #13796, #493, #10797 ) ;
#15372 = CARTESIAN_POINT ( 'NONE',  ( 13.00000000000000178, 4.568735188514060575, 1.737869959597756697 ) ) ;
#15373 = CONICAL_SURFACE ( 'NONE', #2563, 7.937500000000000000, 1.047197551196596521 ) ;
#15374 = ORIENTED_EDGE ( 'NONE', *, *, #10549, .T. ) ;
#15375 = LINE ( 'NONE', #10675, #9989 ) ;
#15376 = ORIENTED_EDGE ( 'NONE', *, *, #12490, .T. ) ;
#15377 = CIRCLE ( 'NONE', #7693, 2.524999999999995914 ) ;
#15378 = EDGE_CURVE ( 'NONE', #62, #18746, #13730, .T. ) ;
#15379 = DIRECTION ( 'NONE',  ( -1.000000000000000000, 1.224646799147353207E-16, 0.000000000000000000 ) ) ;
#15380 = CARTESIAN_POINT ( 'NONE',  ( 13.00000000000000000, -0.2080849974988778772, -4.883670121236158401 ) ) ;
#15381 = CARTESIAN_POINT ( 'NONE',  ( -90.00000000000000000, 0.000000000000000000, 0.000000000000000000 ) ) ;
#15382 = ORIENTED_EDGE ( 'NONE', *, *, #18492, .F. ) ;
#15383 = VERTEX_POINT ( 'NONE', #18241 ) ;
#15384 = CARTESIAN_POINT ( 'NONE',  ( 2.765633920072241292, 18.55949924794916228, -16.37294372382838148 ) ) ;
#15385 = CYLINDRICAL_SURFACE ( 'NONE', #7732, 6.000000000000000000 ) ;
#15386 = VERTEX_POINT ( 'NONE', #4231 ) ;
#15387 = ORIENTED_EDGE ( 'NONE', *, *, #9817, .F. ) ;
#15388 = DIRECTION ( 'NONE',  ( 1.000000000000000000, 0.000000000000000000, 0.000000000000000000 ) ) ;
#15389 = CYLINDRICAL_SURFACE ( 'NONE', #3102, 1.000000000000000888 ) ;
#15390 = LINE ( 'NONE', #12484, #8649 ) ;
#15391 = CYLINDRICAL_SURFACE ( 'NONE', #4546, 1.000000000000002442 ) ;
#15392 = CIRCLE ( 'NONE', #11873, 8.000000000000000000 ) ;
#15393 = CARTESIAN_POINT ( 'NONE',  ( -1.280903732194386802, 4.780397808154273065, -14.34374999795161365 ) ) ;
#15394 = AXIS2_PLACEMENT_3D ( 'NONE', #16009, #11600, #17704 ) ;
#15395 = ORIENTED_EDGE ( 'NONE', *, *, #7936, .T. ) ;
#15396 = EDGE_CURVE ( 'NONE', #16380, #13666, #5734, .T. ) ;
#15397 = CARTESIAN_POINT ( 'NONE',  ( 13.00000000000000178, -4.568735188514048140, -1.737869959597788672 ) ) ;
#15398 = ORIENTED_EDGE ( 'NONE', *, *, #4026, .T. ) ;
#15399 = CARTESIAN_POINT ( 'NONE',  ( 1.749999999999998002, -25.12109765559663188, 12.52377138324213668 ) ) ;
#15400 = CARTESIAN_POINT ( 'NONE',  ( 7.937500000000001776, 3.090998114436798616, -0.3168978725525095075 ) ) ;
#15401 = ADVANCED_FACE ( 'NONE', ( #4519 ), #12237, .T. ) ;
#15402 = DIRECTION ( 'NONE',  ( 0.000000000000000000, 0.000000000000000000, -1.000000000000000000 ) ) ;
#15403 = CARTESIAN_POINT ( 'NONE',  ( 2.765633920072239516, -24.15498966839958683, -5.391175441198872598 ) ) ;
#15404 = VERTEX_POINT ( 'NONE', #13332 ) ;
#15405 = CIRCLE ( 'NONE', #15090, 1.000000000000003109 ) ;
#15406 = CIRCLE ( 'NONE', #11888, 2.524999999999995914 ) ;
#15407 = CARTESIAN_POINT ( 'NONE',  ( 9.000000000000005329, 4.611396867937201272, -3.350375938067097437 ) ) ;
#15408 = DIRECTION ( 'NONE',  ( 0.000000000000000000, 0.000000000000000000, 1.000000000000000000 ) ) ;
#15409 = AXIS2_PLACEMENT_3D ( 'NONE', #207, #8099, #5393 ) ;
#15410 = ORIENTED_EDGE ( 'NONE', *, *, #4150, .F. ) ;
#15411 = DIRECTION ( 'NONE',  ( 1.000000000000000000, 0.000000000000000000, 0.000000000000000000 ) ) ;
#15412 = CYLINDRICAL_SURFACE ( 'NONE', #11607, 2.524999999999995914 ) ;
#15413 = CARTESIAN_POINT ( 'NONE',  ( 10.12500000000000178, 0.000000000000000000, 0.000000000000000000 ) ) ;
#15414 = VECTOR ( 'NONE', #9484, 1000.000000000000000 ) ;
#15415 = CARTESIAN_POINT ( 'NONE',  ( 0.000000000000000000, 25.59481291497571220, 0.000000000000000000 ) ) ;
#15416 = VERTEX_POINT ( 'NONE', #17942 ) ;
#15417 = CARTESIAN_POINT ( 'NONE',  ( 2.789999999999999147, 5.391175441198956086, -24.15498966839956907 ) ) ;
#15418 = CARTESIAN_POINT ( 'NONE',  ( -4.648860486681953397, 1.510506337161861445, -7.843749997951614539 ) ) ;
#15419 = ORIENTED_EDGE ( 'NONE', *, *, #6250, .T. ) ;
#15420 = CARTESIAN_POINT ( 'NONE',  ( 5.500000000000005329, 0.000000000000000000, -32.79058411375427795 ) ) ;
#15421 = EDGE_CURVE ( 'NONE', #16744, #11644, #8933, .T. ) ;
#15422 = FACE_OUTER_BOUND ( 'NONE', #4598, .T. ) ;
#15423 = AXIS2_PLACEMENT_3D ( 'NONE', #15897, #14397, #2180 ) ;
#15424 = ORIENTED_EDGE ( 'NONE', *, *, #3216, .T. ) ;
#15425 = AXIS2_PLACEMENT_3D ( 'NONE', #13967, #258, #13572 ) ;
#15426 = AXIS2_PLACEMENT_3D ( 'NONE', #18581, #19689, #6072 ) ;
#15427 = EDGE_CURVE ( 'NONE', #768, #5986, #12431, .T. ) ;
#15428 = CARTESIAN_POINT ( 'NONE',  ( -2.873153789725825469, 3.954556930911862000, -9.468749997951615427 ) ) ;
#15429 = CARTESIAN_POINT ( 'NONE',  ( 0.000000000000000000, 0.000000000000000000, 0.000000000000000000 ) ) ;
#15430 = EDGE_CURVE ( 'NONE', #3802, #12789, #6601, .T. ) ;
#15431 = ORIENTED_EDGE ( 'NONE', *, *, #8634, .T. ) ;
#15432 = CARTESIAN_POINT ( 'NONE',  ( -7.625032001148274383E-14, 9.515416771311183908, 22.38018801136479397 ) ) ;
#15433 = FACE_OUTER_BOUND ( 'NONE', #8357, .T. ) ;
#15434 = EDGE_LOOP ( 'NONE', ( #7831, #9518, #4460, #4014 ) ) ;
#15435 = CARTESIAN_POINT ( 'NONE',  ( 2.000000000000000000, 1.999999999999997335, 41.99999999999999289 ) ) ;
#15436 = ORIENTED_EDGE ( 'NONE', *, *, #2557, .F. ) ;
#15437 = DIRECTION ( 'NONE',  ( 1.000000000000000000, 0.000000000000000000, 0.000000000000000000 ) ) ;
#15438 = TOROIDAL_SURFACE ( 'NONE', #17038, 6.000000000000000000, 1.199999999999999956 ) ;
#15439 = ORIENTED_EDGE ( 'NONE', *, *, #3671, .F. ) ;
#15440 = DIRECTION ( 'NONE',  ( 0.000000000000000000, 0.000000000000000000, 1.000000000000000000 ) ) ;
#15441 = CARTESIAN_POINT ( 'NONE',  ( -2.695436003842760275, -4.150607464521772094, -10.34374999795161543 ) ) ;
#15442 = ADVANCED_FACE ( 'NONE', ( #421 ), #18334, .F. ) ;
#15443 = DIRECTION ( 'NONE',  ( 0.000000000000000000, 0.000000000000000000, 1.000000000000000000 ) ) ;
#15444 = VECTOR ( 'NONE', #3532, 1000.000000000000000 ) ;
#15445 = CARTESIAN_POINT ( 'NONE',  ( 11.46874999795161543, 2.444050593749990785, 4.233219804643887585 ) ) ;
#15446 = ORIENTED_EDGE ( 'NONE', *, *, #16808, .F. ) ;
#15447 = VECTOR ( 'NONE', #1509, 1000.000000000000000 ) ;
#15448 = DIRECTION ( 'NONE',  ( 0.000000000000000000, 0.000000000000000000, -1.000000000000000000 ) ) ;
#15449 = EDGE_CURVE ( 'NONE', #1278, #18746, #10553, .T. ) ;
#15450 = DIRECTION ( 'NONE',  ( 1.000000000000000000, -0.000000000000000000, -0.000000000000000000 ) ) ;
#15451 = ADVANCED_FACE ( 'NONE', ( #9533 ), #4822, .F. ) ;
#15452 = STYLED_ITEM ( 'NONE', ( #1301 ), #2068 ) ;
#15453 = FACE_OUTER_BOUND ( 'NONE', #16248, .T. ) ;
#15454 = DIRECTION ( 'NONE',  ( 0.000000000000000000, -1.000000000000000000, 0.000000000000000000 ) ) ;
#15455 = CARTESIAN_POINT ( 'NONE',  ( 17.28688694438834972, -7.664027248171309203, -35.00000000000000000 ) ) ;
#15456 = ORIENTED_EDGE ( 'NONE', *, *, #12016, .T. ) ;
#15457 = CARTESIAN_POINT ( 'NONE',  ( -7.937500000000000000, -4.582717761692662428, -6.527800000000000047 ) ) ;
#15458 = DIRECTION ( 'NONE',  ( 0.000000000000000000, 0.000000000000000000, 1.000000000000000000 ) ) ;
#15459 = AXIS2_PLACEMENT_3D ( 'NONE', #8701, #11704, #910 ) ;
#15460 = ORIENTED_EDGE ( 'NONE', *, *, #4889, .T. ) ;
#15461 = CARTESIAN_POINT ( 'NONE',  ( 12.99999999999998401, 0.02830770314434387022, -5.175540411820488629 ) ) ;
#15462 = ORIENTED_EDGE ( 'NONE', *, *, #8979, .T. ) ;
#15463 = PRODUCT_CONTEXT ( 'NONE', #3680, 'mechanical' ) ;
#15464 = LINE ( 'NONE', #16868, #87 ) ;
#15465 = CARTESIAN_POINT ( 'NONE',  ( 7.468749997951615427, 4.781284448697194378, -1.016293382781411125 ) ) ;
#15466 = ADVANCED_FACE ( 'NONE', ( #4724 ), #17889, .T. ) ;
#15467 = ORIENTED_EDGE ( 'NONE', *, *, #14468, .T. ) ;
#15468 = ORIENTED_EDGE ( 'NONE', *, *, #9329, .F. ) ;
#15469 = DIRECTION ( 'NONE',  ( 0.000000000000000000, 0.000000000000000000, -1.000000000000000000 ) ) ;
#15470 = CARTESIAN_POINT ( 'NONE',  ( -1.016293382781411569, 4.781284448697194378, -7.843749997951614539 ) ) ;
#15471 = ORIENTED_EDGE ( 'NONE', *, *, #15203, .T. ) ;
#15472 =( BOUNDED_SURFACE ( )  B_SPLINE_SURFACE ( 1, 2, ( 
 ( #19325, #17935, #745, #7201, #6919, #8537, #17832, #16436, #6822, #4126, #19425, #9953, #5709, #14645, #5332, #10140, #11826 ),
 ( #13134, #11445, #19230, #10238, #16332, #17545, #2330, #14549, #842, #5424, #2713, #16044, #11536, #8625, #11730, #3931, #14447 ) ),
 .UNSPECIFIED., .F., .F., .F. ) 
 B_SPLINE_SURFACE_WITH_KNOTS ( ( 2, 2 ),
 ( 3, 2, 2, 2, 2, 2, 2, 2, 3 ),
 ( 0.000000000000000000, 1.000000000000000000 ),
 ( 0.000000000000000000, 0.05000000000000000278, 0.1000000000000000056, 0.1499999999999999944, 0.2000000000000000111, 0.2500000000000000000, 0.2999999999999999889, 0.3499999999999999778, 0.4000000000000000222 ),
 .UNSPECIFIED. ) 
 GEOMETRIC_REPRESENTATION_ITEM ( )  RATIONAL_B_SPLINE_SURFACE ( (
 ( 1.000000000000000000, 0.9876883405951377704, 1.000000000000000000, 0.9876883405951377704, 1.000000000000000000, 0.9876883405951377704, 1.000000000000000000, 0.9876883405951377704, 1.000000000000000000, 0.9876883405951377704, 1.000000000000000000, 0.9876883405951377704, 1.000000000000000000, 0.9876883405951377704, 1.000000000000000000, 0.9876883405951377704, 1.000000000000000000),
 ( 1.000000000000000000, 0.9876883405951377704, 1.000000000000000000, 0.9876883405951377704, 1.000000000000000000, 0.9876883405951377704, 1.000000000000000000, 0.9876883405951377704, 1.000000000000000000, 0.9876883405951377704, 1.000000000000000000, 0.9876883405951377704, 1.000000000000000000, 0.9876883405951377704, 1.000000000000000000, 0.9876883405951377704, 1.000000000000000000) ) ) 
 REPRESENTATION_ITEM ( '' )  SURFACE ( )  );
#15473 = EDGE_CURVE ( 'NONE', #3050, #15740, #11128, .T. ) ;
#15474 = CARTESIAN_POINT ( 'NONE',  ( 0.000000000000000000, 24.34211360614300190, 7.909232158574900140 ) ) ;
#15475 = ORIENTED_EDGE ( 'NONE', *, *, #8822, .T. ) ;
#15476 = AXIS2_PLACEMENT_3D ( 'NONE', #14048, #15556, #6232 ) ;
#15477 = CARTESIAN_POINT ( 'NONE',  ( 11.96874999795161365, -1.773574444220693325, -4.620319390059841602 ) ) ;
#15478 = DIRECTION ( 'NONE',  ( -1.000000000000000000, -0.000000000000000000, -0.000000000000000000 ) ) ;
#15479 = CARTESIAN_POINT ( 'NONE',  ( 13.00000000000000178, -0.5236311934647339683, -4.860400829920959787 ) ) ;
#15480 = CARTESIAN_POINT ( 'NONE',  ( 2.765633920072239071, -12.59161484032927092, 21.30679549418627161 ) ) ;
#15481 = ORIENTED_EDGE ( 'NONE', *, *, #10428, .T. ) ;
#15482 = CARTESIAN_POINT ( 'NONE',  ( 0.000000000000000000, 0.000000000000000000, -6.000000000000005329 ) ) ;
#15483 = FILL_AREA_STYLE_COLOUR ( '', #9078 ) ;
#15484 = AXIS2_PLACEMENT_3D ( 'NONE', #3615, #3714, #11124 ) ;
#15485 = ADVANCED_FACE ( 'NONE', ( #10732 ), #16843, .F. ) ;
#15486 = ORIENTED_EDGE ( 'NONE', *, *, #3718, .T. ) ;
#15487 = ORIENTED_EDGE ( 'NONE', *, *, #8136, .T. ) ;
#15488 = CARTESIAN_POINT ( 'NONE',  ( -41.99999999999999289, 4.999999999999998224, 2.000000000000000000 ) ) ;
#15489 = DIRECTION ( 'NONE',  ( 1.000000000000000000, 0.000000000000000000, 0.000000000000000000 ) ) ;
#15490 = DIRECTION ( 'NONE',  ( -1.000000000000000000, -0.000000000000000000, 0.000000000000000000 ) ) ;
#15491 = DIRECTION ( 'NONE',  ( 1.000000000000000000, 0.000000000000000000, 0.000000000000000000 ) ) ;
#15492 =( GEOMETRIC_REPRESENTATION_CONTEXT ( 3 ) GLOBAL_UNCERTAINTY_ASSIGNED_CONTEXT ( ( #7361 ) ) GLOBAL_UNIT_ASSIGNED_CONTEXT ( ( #2300, #17708, #14522 ) ) REPRESENTATION_CONTEXT ( 'NONE', 'WORKASPACE' ) );
#15493 = CARTESIAN_POINT ( 'NONE',  ( -36.00000000000000000, -2.311115933264683024E-31, 0.000000000000000000 ) ) ;
#15494 = EDGE_CURVE ( 'NONE', #870, #9786, #3837, .T. ) ;
#15495 = ORIENTED_EDGE ( 'NONE', *, *, #8983, .F. ) ;
#15496 = DIRECTION ( 'NONE',  ( 0.000000000000000000, 0.000000000000000000, 1.000000000000000000 ) ) ;
#15497 = LINE ( 'NONE', #7974, #15238 ) ;
#15498 = VERTEX_POINT ( 'NONE', #9436 ) ;
#15499 = CARTESIAN_POINT ( 'NONE',  ( 6.000000000000005329, -4.936344801571268093, -2.850000000000058265 ) ) ;
#15500 = CIRCLE ( 'NONE', #6849, 1.000000000000000888 ) ;
#15501 = CARTESIAN_POINT ( 'NONE',  ( 0.1882238782932339760, -19.18368891937503307, 17.47009390565483855 ) ) ;
#15502 = EDGE_CURVE ( 'NONE', #5836, #13251, #15980, .T. ) ;
#15503 = DIRECTION ( 'NONE',  ( -1.000000000000000000, -1.224646799147353207E-16, -0.000000000000000000 ) ) ;
#15504 = DIRECTION ( 'NONE',  ( 0.000000000000000000, 0.000000000000000000, -1.000000000000000000 ) ) ;
#15505 = CARTESIAN_POINT ( 'NONE',  ( -4.080749450109677490, -4.080749450109621534, -13.50000000000000533 ) ) ;
#15506 = ORIENTED_EDGE ( 'NONE', *, *, #8803, .F. ) ;
#15507 = TOROIDAL_SURFACE ( 'NONE', #11988, 24.12539914357697768, 8.000000000000000000 ) ;
#15508 = CARTESIAN_POINT ( 'NONE',  ( 1.894355403937850069, -24.59653223688283674, 12.96989951879399072 ) ) ;
#15509 = CARTESIAN_POINT ( 'NONE',  ( -90.00000000000000000, 0.000000000000000000, -6.735000000000022524 ) ) ;
#15510 = DIRECTION ( 'NONE',  ( 1.000000000000000000, 6.419766481290786633E-33, -0.000000000000000000 ) ) ;
#15511 = ORIENTED_EDGE ( 'NONE', *, *, #7498, .F. ) ;
#15512 = DIRECTION ( 'NONE',  ( 0.000000000000000000, -1.000000000000000000, 0.000000000000000000 ) ) ;
#15513 = CARTESIAN_POINT ( 'NONE',  ( 8.000000000000005329, 5.668774803599156975, 0.5958122406256382009 ) ) ;
#15514 = DIRECTION ( 'NONE',  ( 1.000000000000000000, 0.000000000000000000, 0.000000000000000000 ) ) ;
#15515 = ORIENTED_EDGE ( 'NONE', *, *, #6539, .T. ) ;
#15516 = CARTESIAN_POINT ( 'NONE',  ( 1.039999999999997593, 0.000000000000000000, 0.000000000000000000 ) ) ;
#15517 = DIRECTION ( 'NONE',  ( -1.000000000000000000, -0.000000000000000000, -0.000000000000000000 ) ) ;
#15518 = EDGE_CURVE ( 'NONE', #13685, #9061, #16307, .T. ) ;
#15519 = ORIENTED_EDGE ( 'NONE', *, *, #7465, .F. ) ;
#15520 = CYLINDRICAL_SURFACE ( 'NONE', #12522, 13.19999999999999929 ) ;
#15521 = CARTESIAN_POINT ( 'NONE',  ( 16.11901729331276556, 5.562305898749055011, -35.00000000000000000 ) ) ;
#15522 = AXIS2_PLACEMENT_3D ( 'NONE', #2436, #6933, #6732 ) ;
#15523 = ORIENTED_EDGE ( 'NONE', *, *, #15186, .F. ) ;
#15524 = AXIS2_PLACEMENT_3D ( 'NONE', #17874, #4268, #2655 ) ;
#15525 =( BOUNDED_SURFACE ( )  B_SPLINE_SURFACE ( 1, 2, ( 
 ( #9105, #15103, #2685, #5782, #15306, #12001, #7373, #4198, #7175, #10311, #19494, #13396, #15205, #7581, #16408, #10408, #13495 ),
 ( #16508, #18106, #6081, #7785, #12599, #18397, #1786, #13997, #17003, #1884, #7978, #18787, #10993, #91, #6276, #7682, #12495 ) ),
 .UNSPECIFIED., .F., .F., .T. ) 
 B_SPLINE_SURFACE_WITH_KNOTS ( ( 2, 2 ),
 ( 3, 2, 2, 2, 2, 2, 2, 2, 3 ),
 ( 0.000000000000000000, 1.000000000000000000 ),
 ( 0.000000000000000000, 0.05000000000000000278, 0.1000000000000000056, 0.1499999999999999944, 0.2000000000000000111, 0.2500000000000000000, 0.2999999999999999889, 0.3499999999999999778, 0.4000000000000000222 ),
 .UNSPECIFIED. ) 
 GEOMETRIC_REPRESENTATION_ITEM ( )  RATIONAL_B_SPLINE_SURFACE ( (
 ( 1.000000000000000000, 0.9876883405951377704, 1.000000000000000000, 0.9876883405951377704, 1.000000000000000000, 0.9876883405951377704, 1.000000000000000000, 0.9876883405951377704, 1.000000000000000000, 0.9876883405951377704, 1.000000000000000000, 0.9876883405951377704, 1.000000000000000000, 0.9876883405951377704, 1.000000000000000000, 0.9876883405951377704, 1.000000000000000000),
 ( 1.000000000000000000, 0.9876883405951377704, 1.000000000000000000, 0.9876883405951377704, 1.000000000000000000, 0.9876883405951377704, 1.000000000000000000, 0.9876883405951377704, 1.000000000000000000, 0.9876883405951377704, 1.000000000000000000, 0.9876883405951377704, 1.000000000000000000, 0.9876883405951377704, 1.000000000000000000, 0.9876883405951377704, 1.000000000000000000) ) ) 
 REPRESENTATION_ITEM ( '' )  SURFACE ( )  );
#15526 = CARTESIAN_POINT ( 'NONE',  ( -16.68117051311640253, -3.372863662543042818, 32.00000000000000000 ) ) ;
#15527 = CARTESIAN_POINT ( 'NONE',  ( -16.28688694438836038, -7.664027248171298545, 35.00000000000000000 ) ) ;
#15528 = VERTEX_POINT ( 'NONE', #9331 ) ;
#15529 = DIRECTION ( 'NONE',  ( 0.000000000000000000, 0.000000000000000000, -1.000000000000000000 ) ) ;
#15530 = CARTESIAN_POINT ( 'NONE',  ( 2.299999999999996270, 7.347880794884145374E-16, 6.000000000000021316 ) ) ;
#15531 = ORIENTED_EDGE ( 'NONE', *, *, #11763, .F. ) ;
#15532 = EDGE_CURVE ( 'NONE', #7717, #2446, #2236, .T. ) ;
#15533 = DIRECTION ( 'NONE',  ( -9.559896011775280412E-17, -0.7806247497997995666, -0.6250000000000002220 ) ) ;
#15534 = ORIENTED_EDGE ( 'NONE', *, *, #13869, .F. ) ;
#15535 = ADVANCED_FACE ( 'NONE', ( #1915 ), #3221, .F. ) ;
#15536 = DIRECTION ( 'NONE',  ( -1.000000000000000000, 0.000000000000000000, -0.000000000000000000 ) ) ;
#15537 = AXIS2_PLACEMENT_3D ( 'NONE', #5013, #6304, #17224 ) ;
#15538 = ORIENTED_EDGE ( 'NONE', *, *, #8690, .T. ) ;
#15539 = DIRECTION ( 'NONE',  ( -1.000000000000000000, -0.000000000000000000, -0.000000000000000000 ) ) ;
#15540 = AXIS2_PLACEMENT_3D ( 'NONE', #2007, #9620, #8207 ) ;
#15541 = CARTESIAN_POINT ( 'NONE',  ( -1.988169868018624609, -4.465502636338009701, -9.843749997951615427 ) ) ;
#15542 = CYLINDRICAL_SURFACE ( 'NONE', #11682, 1.000000000000002665 ) ;
#15543 = CARTESIAN_POINT ( 'NONE',  ( 2.444050593750020095, 4.233219804643871598, -6.468749997951615427 ) ) ;
#15544 = VERTEX_POINT ( 'NONE', #10930 ) ;
#15545 = FACE_OUTER_BOUND ( 'NONE', #18244, .T. ) ;
#15546 = CARTESIAN_POINT ( 'NONE',  ( 2.790000000000079527, 18.34439787333507255, 15.96555658743769079 ) ) ;
#15547 = VECTOR ( 'NONE', #13303, 1000.000000000000000 ) ;
#15548 = VERTEX_POINT ( 'NONE', #9234 ) ;
#15549 = VECTOR ( 'NONE', #10206, 1000.000000000000000 ) ;
#15550 = CARTESIAN_POINT ( 'NONE',  ( -5.207209108562804722, 2.318398865532109276, -14.00000000000000533 ) ) ;
#15551 = CARTESIAN_POINT ( 'NONE',  ( 2.789999999999999147, -5.535312321042557215, -23.48180575137735815 ) ) ;
#15552 = ORIENTED_EDGE ( 'NONE', *, *, #17641, .T. ) ;
#15553 = CARTESIAN_POINT ( 'NONE',  ( 9.500000000000005329, -4.840010801796461593, -3.143139765844656264 ) ) ;
#15554 = DIRECTION ( 'NONE',  ( 1.000000000000000000, 0.000000000000000000, 0.000000000000000000 ) ) ;
#15555 = VERTEX_POINT ( 'NONE', #15340 ) ;
#15556 = DIRECTION ( 'NONE',  ( -1.000000000000000000, 0.000000000000000000, 0.000000000000000000 ) ) ;
#15557 = ORIENTED_EDGE ( 'NONE', *, *, #6095, .F. ) ;
#15558 = PRODUCT_CONTEXT ( 'NONE', #12132, 'mechanical' ) ;
#15559 = DIRECTION ( 'NONE',  ( 1.000000000000000000, 0.000000000000000000, 0.000000000000000000 ) ) ;
#15560 = CARTESIAN_POINT ( 'NONE',  ( 13.96874999795161365, -1.280903732194453859, 4.780397808154257078 ) ) ;
#15561 = ORIENTED_EDGE ( 'NONE', *, *, #16385, .T. ) ;
#15562 = VERTEX_POINT ( 'NONE', #11028 ) ;
#15563 = FACE_OUTER_BOUND ( 'NONE', #9743, .T. ) ;
#15564 = VECTOR ( 'NONE', #19637, 1000.000000000000000 ) ;
#15565 = B_SPLINE_CURVE_WITH_KNOTS ( 'NONE', 3,
 ( #17992, #18088, #5670, #2567 ),
 .UNSPECIFIED., .F., .F.,
 ( 4, 4 ),
 ( 0.0006045424356927869836, 0.0006887909409525213005 ),
 .UNSPECIFIED. ) ;
#15566 = AXIS2_PLACEMENT_3D ( 'NONE', #15415, #1709, #7799 ) ;
#15567 = ORIENTED_EDGE ( 'NONE', *, *, #11649, .F. ) ;
#15568 = ADVANCED_FACE ( 'NONE', ( #8118 ), #14227, .T. ) ;
#15569 = ADVANCED_FACE ( 'NONE', ( #7716 ), #12337, .F. ) ;
#15570 = DIRECTION ( 'NONE',  ( 0.000000000000000000, -1.000000000000000000, 0.000000000000000000 ) ) ;
#15571 = VERTEX_POINT ( 'NONE', #6803 ) ;
#15572 = AXIS2_PLACEMENT_3D ( 'NONE', #11812, #7491, #2997 ) ;
#15573 = CARTESIAN_POINT ( 'NONE',  ( 13.96874999795161365, 1.280903732194486722, -4.780397808154247308 ) ) ;
#15574 = AXIS2_PLACEMENT_3D ( 'NONE', #1857, #3549, #3358 ) ;
#15575 = DIRECTION ( 'NONE',  ( -1.000000000000000000, -0.000000000000000000, -0.000000000000000000 ) ) ;
#15576 = FACE_BOUND ( 'NONE', #656, .T. ) ;
#15577 = ORIENTED_EDGE ( 'NONE', *, *, #7099, .T. ) ;
#15578 = LINE ( 'NONE', #12475, #1508 ) ;
#15579 = EDGE_CURVE ( 'NONE', #3194, #4661, #15828, .T. ) ;
#15580 = DIRECTION ( 'NONE',  ( 0.000000000000000000, 0.000000000000000000, -1.000000000000000000 ) ) ;
#15581 = VERTEX_POINT ( 'NONE', #5504 ) ;
#15582 = EDGE_LOOP ( 'NONE', ( #6, #7579, #7598, #8635 ) ) ;
#15583 = B_SPLINE_CURVE_WITH_KNOTS ( 'NONE', 1,
 ( #17521, #2496 ),
 .UNSPECIFIED., .F., .F.,
 ( 2, 2 ),
 ( 0.000000000000000000, 1.000000000000000000 ),
 .UNSPECIFIED. ) ;
#15584 = DIRECTION ( 'NONE',  ( 0.000000000000000000, 0.000000000000000000, 1.000000000000000000 ) ) ;
#15585 = CARTESIAN_POINT ( 'NONE',  ( -2.318398865532109721, -5.207209108562803834, -10.31249999590322552 ) ) ;
#15586 = DIRECTION ( 'NONE',  ( -1.000000000000000000, -0.000000000000000000, -0.000000000000000000 ) ) ;
#15587 = DIRECTION ( 'NONE',  ( 0.000000000000000000, 0.000000000000000000, 1.000000000000000000 ) ) ;
#15588 = AXIS2_PLACEMENT_3D ( 'NONE', #12412, #4799, #10905 ) ;
#15589 = DIRECTION ( 'NONE',  ( 0.000000000000000000, -1.000000000000000000, 0.000000000000000000 ) ) ;
#15590 = AXIS2_PLACEMENT_3D ( 'NONE', #8327, #833, #735 ) ;
#15591 = VERTEX_POINT ( 'NONE', #9839 ) ;
#15592 = CARTESIAN_POINT ( 'NONE',  ( 0.000000000000000000, 1.224646799147353256E-15, -10.00000000000000000 ) ) ;
#15593 = CARTESIAN_POINT ( 'NONE',  ( 12.92161831991541554, -4.611601942845651614, -1.625176344145968788 ) ) ;
#15594 = EDGE_LOOP ( 'NONE', ( #18365, #6015, #10758, #15997, #15387, #891 ) ) ;
#15595 = DIRECTION ( 'NONE',  ( 1.000000000000000000, 0.000000000000000000, 0.000000000000000000 ) ) ;
#15596 = EDGE_CURVE ( 'NONE', #9581, #5937, #9740, .T. ) ;
#15597 = CARTESIAN_POINT ( 'NONE',  ( -2.255998204157477538, -17.85806462366060288, 32.00000000000000000 ) ) ;
#15598 = CARTESIAN_POINT ( 'NONE',  ( 17.68117051311639898, -3.372863662543048591, 32.00000000000000000 ) ) ;
#15599 = DIRECTION ( 'NONE',  ( 0.000000000000000000, 0.000000000000000000, 1.000000000000000000 ) ) ;
#15600 = DIRECTION ( 'NONE',  ( 0.000000000000000000, -0.7315216790650493905, 0.6818181818181815457 ) ) ;
#15601 = VERTEX_POINT ( 'NONE', #11517 ) ;
#15602 = AXIS2_PLACEMENT_3D ( 'NONE', #3195, #202, #6284 ) ;
#15603 = CYLINDRICAL_SURFACE ( 'NONE', #5328, 1.000000000000000000 ) ;
#15604 = CARTESIAN_POINT ( 'NONE',  ( 2.299999999999996270, 1.102182119232620672E-15, 9.000000000000021316 ) ) ;
#15605 = AXIS2_PLACEMENT_3D ( 'NONE', #6292, #12418, #5004 ) ;
#15606 =( NAMED_UNIT ( * ) SI_UNIT ( $, .STERADIAN. ) SOLID_ANGLE_UNIT ( ) );
#15607 = EDGE_LOOP ( 'NONE', ( #17850, #18563, #8734, #2296 ) ) ;
#15608 = DIRECTION ( 'NONE',  ( 0.000000000000000000, -0.000000000000000000, 1.000000000000000000 ) ) ;
#15609 = CARTESIAN_POINT ( 'NONE',  ( 0.02436607992776411782, -24.63872515616084513, 2.336989772644183283 ) ) ;
#15610 = CARTESIAN_POINT ( 'NONE',  ( 13.46874999795161543, -0.5109457054261780096, 4.861323657744406113 ) ) ;
#15611 = CARTESIAN_POINT ( 'NONE',  ( -34.92499999999994742, 7.347880794884119736E-16, -6.000000000000000000 ) ) ;
#15612 = DIRECTION ( 'NONE',  ( -1.000000000000000000, -0.000000000000000000, -0.000000000000000000 ) ) ;
#15613 = VERTEX_POINT ( 'NONE', #10032 ) ;
#15614 = CARTESIAN_POINT ( 'NONE',  ( -17.11901729331276911, 5.562305898749051458, 32.00000000000000000 ) ) ;
#15615 = CARTESIAN_POINT ( 'NONE',  ( 1.510506337161861223, 4.648860486681953397, -12.84374999795161543 ) ) ;
#15616 = EDGE_LOOP ( 'NONE', ( #5909, #11986 ) ) ;
#15617 = CARTESIAN_POINT ( 'NONE',  ( 13.46874999795161543, -3.954556930911842016, -2.873153789725852558 ) ) ;
#15618 = DIRECTION ( 'NONE',  ( 0.000000000000000000, 0.000000000000000000, 1.000000000000000000 ) ) ;
#15619 = VECTOR ( 'NONE', #4461, 1000.000000000000000 ) ;
#15620 = ORIENTED_EDGE ( 'NONE', *, *, #17053, .F. ) ;
#15621 = EDGE_CURVE ( 'NONE', #768, #5267, #5409, .T. ) ;
#15622 = B_SPLINE_CURVE_WITH_KNOTS ( 'NONE', 3,
 ( #9537, #15636, #3621, #5114, #3328, #4827 ),
 .UNSPECIFIED., .F., .F.,
 ( 4, 2, 4 ),
 ( 1.979325885420663486E-07, 0.001878588715165609938, 0.003756979497742677504 ),
 .UNSPECIFIED. ) ;
#15623 = AXIS2_PLACEMENT_3D ( 'NONE', #1457, #1357, #15061 ) ;
#15624 = LINE ( 'NONE', #12721, #700 ) ;
#15625 = DIRECTION ( 'NONE',  ( -1.000000000000000000, 0.000000000000000000, 0.000000000000000000 ) ) ;
#15626 = ORIENTED_EDGE ( 'NONE', *, *, #11729, .F. ) ;
#15627 = CARTESIAN_POINT ( 'NONE',  ( 2.601776105308175602, -25.78859396478526023, -2.857713464478961463 ) ) ;
#15628 = DIRECTION ( 'NONE',  ( 0.000000000000000000, 0.000000000000000000, 1.000000000000000000 ) ) ;
#15629 = ADVANCED_FACE ( 'NONE', ( #18922 ), #14719, .T. ) ;
#15630 = VERTEX_POINT ( 'NONE', #16133 ) ;
#15631 = CARTESIAN_POINT ( 'NONE',  ( -19.00000000000000355, -3.278623949159157558, -2.625000000000002220 ) ) ;
#15632 = ORIENTED_EDGE ( 'NONE', *, *, #3825, .T. ) ;
#15634 = CARTESIAN_POINT ( 'NONE',  ( 1.394999999999998685, -4.147968289691093879, -27.76164181293055933 ) ) ;
#15633 = AXIS2_PLACEMENT_3D ( 'NONE', #17166, #761, #15662 ) ;
#15635 = EDGE_LOOP ( 'NONE', ( #568, #6522, #13461, #9381, #16545, #7914 ) ) ;
#15636 = CARTESIAN_POINT ( 'NONE',  ( 2.718131847775119514, -5.344160105508880321, 24.78765742476137035 ) ) ;
#15637 = CARTESIAN_POINT ( 'NONE',  ( 8.671566133830875600, 15.77352024078954784, -32.00000000000000000 ) ) ;
#15638 = CARTESIAN_POINT ( 'NONE',  ( -5.574407415329178939, -1.493657965219446160, -8.500000000000005329 ) ) ;
#15639 = CARTESIAN_POINT ( 'NONE',  ( 3.114526743279282694, 3.846120219227923798, -6.968749997951614539 ) ) ;
#15640 = ORIENTED_EDGE ( 'NONE', *, *, #13998, .T. ) ;
#15641 = ORIENTED_EDGE ( 'NONE', *, *, #12981, .F. ) ;
#15642 = CARTESIAN_POINT ( 'NONE',  ( 2.765633920072234631, -21.30679549418640306, 12.59161484032904887 ) ) ;
#15643 = SHAPE_REPRESENTATION ( 'brake arm', ( #16724 ), #2332 ) ;
#15644 = CARTESIAN_POINT ( 'NONE',  ( 0.000000000000000000, 0.000000000000000000, 0.000000000000000000 ) ) ;
#15645 = VERTEX_POINT ( 'NONE', #8221 ) ;
#15646 = CARTESIAN_POINT ( 'NONE',  ( -41.99999999999999289, 1.999999999999998224, -5.000000000000000000 ) ) ;
#15647 = DIRECTION ( 'NONE',  ( -1.000000000000000000, 0.000000000000000000, -0.000000000000000000 ) ) ;
#15648 = DIRECTION ( 'NONE',  ( 1.000000000000000000, 0.000000000000000000, 0.000000000000000000 ) ) ;
#15649 = ORIENTED_EDGE ( 'NONE', *, *, #5059, .T. ) ;
#15651 = CARTESIAN_POINT ( 'NONE',  ( 1.749999999999998002, 27.68468304288265358, -4.633866840648635410 ) ) ;
#15650 =( GEOMETRIC_REPRESENTATION_CONTEXT ( 3 ) GLOBAL_UNCERTAINTY_ASSIGNED_CONTEXT ( ( #7165 ) ) GLOBAL_UNIT_ASSIGNED_CONTEXT ( ( #5847, #16774, #8866 ) ) REPRESENTATION_CONTEXT ( 'NONE', 'WORKASPACE' ) );
#15652 = DIRECTION ( 'NONE',  ( 0.000000000000000000, -3.552713678800500929E-15, 1.000000000000000000 ) ) ;
#15653 = EDGE_CURVE ( 'NONE', #62, #2117, #965, .T. ) ;
#15654 = ORIENTED_EDGE ( 'NONE', *, *, #13594, .T. ) ;
#15655 = CYLINDRICAL_SURFACE ( 'NONE', #11328, 5.700000000000001954 ) ;
#15656 = ORIENTED_EDGE ( 'NONE', *, *, #17938, .T. ) ;
#15657 = PRODUCT_CONTEXT ( 'NONE', #11487, 'mechanical' ) ;
#15658 = CARTESIAN_POINT ( 'NONE',  ( 2.500000000000002220, 0.000000000000000000, 6.543750000000017941 ) ) ;
#15659 = CARTESIAN_POINT ( 'NONE',  ( 8.968749997951611874, 4.780397808154257078, 1.280903732194454303 ) ) ;
#15660 = ORIENTED_EDGE ( 'NONE', *, *, #6826, .F. ) ;
#15661 = ORIENTED_EDGE ( 'NONE', *, *, #18759, .T. ) ;
#15662 = DIRECTION ( 'NONE',  ( 0.000000000000000000, 0.000000000000000000, 1.000000000000000000 ) ) ;
#15663 = PLANE ( 'NONE',  #15574 ) ;
#15664 = ORIENTED_EDGE ( 'NONE', *, *, #408, .T. ) ;
#15665 =( GEOMETRIC_REPRESENTATION_CONTEXT ( 3 ) GLOBAL_UNCERTAINTY_ASSIGNED_CONTEXT ( ( #10198 ) ) GLOBAL_UNIT_ASSIGNED_CONTEXT ( ( #7311, #4238, #11938 ) ) REPRESENTATION_CONTEXT ( 'NONE', 'WORKASPACE' ) );
#15666 = VECTOR ( 'NONE', #6115, 1000.000000000000000 ) ;
#15667 = CARTESIAN_POINT ( 'NONE',  ( -0.5109457054261112852, 4.861323657744413218, -14.84374999795161543 ) ) ;
#15668 = EDGE_CURVE ( 'NONE', #5937, #17326, #3187, .T. ) ;
#15669 = EDGE_LOOP ( 'NONE', ( #4559, #15848, #19578, #11973 ) ) ;
#15670 = EDGE_CURVE ( 'NONE', #6802, #10667, #8317, .T. ) ;
#15671 = CARTESIAN_POINT ( 'NONE',  ( 14.46874999795161720, 1.988169868018623720, -4.465502636338010589 ) ) ;
#15672 = CARTESIAN_POINT ( 'NONE',  ( -5.294050593750000644, 0.000000000000000000, -6.234374998975811266 ) ) ;
#15673 = FACE_BOUND ( 'NONE', #18509, .T. ) ;
#15674 = EDGE_CURVE ( 'NONE', #5246, #10962, #324, .T. ) ;
#15675 = VERTEX_POINT ( 'NONE', #5314 ) ;
#15676 = CARTESIAN_POINT ( 'NONE',  ( 13.00000000000000178, 1.070668164103456110, 5.063333171156721768 ) ) ;
#15677 = FILL_AREA_STYLE ('',( #15483 ) ) ;
#15678 = FACE_OUTER_BOUND ( 'NONE', #10111, .T. ) ;
#15679 = ORIENTED_EDGE ( 'NONE', *, *, #17156, .F. ) ;
#15680 = ORIENTED_EDGE ( 'NONE', *, *, #650, .T. ) ;
#15681 = DIRECTION ( 'NONE',  ( 0.000000000000000000, 0.000000000000000000, -1.000000000000000000 ) ) ;
#15682 = EDGE_CURVE ( 'NONE', #8042, #19358, #17327, .T. ) ;
#15683 = CARTESIAN_POINT ( 'NONE',  ( 2.783068930044319877, -16.17493693894864393, -18.43696893154776006 ) ) ;
#15684 = CARTESIAN_POINT ( 'NONE',  ( -2.695436003842674566, 4.150607464521828938, -13.34374999795161365 ) ) ;
#15685 = ORIENTED_EDGE ( 'NONE', *, *, #14634, .T. ) ;
#15686 = DIRECTION ( 'NONE',  ( 1.000000000000000000, 0.000000000000000000, 0.000000000000000000 ) ) ;
#15687 = CARTESIAN_POINT ( 'NONE',  ( 7.312499995903225525, -4.936344801571268093, -2.850000000000058265 ) ) ;
#15688 = CIRCLE ( 'NONE', #14411, 0.1999999999999996503 ) ;
#15689 = ORIENTED_EDGE ( 'NONE', *, *, #6148, .T. ) ;
#15690 = CARTESIAN_POINT ( 'NONE',  ( 11.00000000000000711, 2.850000000000057820, -4.936344801571268093 ) ) ;
#15691 = EDGE_CURVE ( 'NONE', #2239, #12398, #5431, .T. ) ;
#15692 = LINE ( 'NONE', #1982, #4175 ) ;
#15693 = LINE ( 'NONE', #14293, #18929 ) ;
#15694 = CARTESIAN_POINT ( 'NONE',  ( -15.19790265903627180, 9.644882309621941374, -32.00000000000000000 ) ) ;
#15695 = CARTESIAN_POINT ( 'NONE',  ( -2.873153789725852558, -3.954556930911842016, -13.46874999795161543 ) ) ;
#15696 = ORIENTED_EDGE ( 'NONE', *, *, #9198, .T. ) ;
#15697 = FACE_OUTER_BOUND ( 'NONE', #15434, .T. ) ;
#15698 = FILL_AREA_STYLE ('',( #18499 ) ) ;
#15699 = CYLINDRICAL_SURFACE ( 'NONE', #12301, 0.9999999999999974465 ) ;
#15700 =( LENGTH_UNIT ( ) NAMED_UNIT ( * ) SI_UNIT ( .MILLI., .METRE. ) );
#15701 = ORIENTED_EDGE ( 'NONE', *, *, #18008, .F. ) ;
#15702 = LINE ( 'NONE', #8092, #3772 ) ;
#15703 = CONICAL_SURFACE ( 'NONE', #1317, 6.543750000000017941, 0.3653297453805220418 ) ;
#15704 = DIRECTION ( 'NONE',  ( -0.000000000000000000, 0.000000000000000000, 1.000000000000000000 ) ) ;
#15705 = AXIS2_PLACEMENT_3D ( 'NONE', #31, #3866, #7524 ) ;
#15706 = DIRECTION ( 'NONE',  ( 1.000000000000000000, 0.000000000000000000, 0.000000000000000000 ) ) ;
#15707 = ADVANCED_FACE ( 'NONE', ( #8425 ), #14327, .F. ) ;
#15708 = VECTOR ( 'NONE', #7518, 1000.000000000000000 ) ;
#15709 = LINE ( 'NONE', #13810, #19710 ) ;
#15710 = CARTESIAN_POINT ( 'NONE',  ( -7.671566133830872047, 15.77352024078954429, -32.00000000000000000 ) ) ;
#15711 = ORIENTED_EDGE ( 'NONE', *, *, #18807, .T. ) ;
#15712 = CARTESIAN_POINT ( 'NONE',  ( -2.300000000000000711, 0.000000000000000000, -8.800000000000022027 ) ) ;
#15713 = CARTESIAN_POINT ( 'NONE',  ( 16.28688694438835327, -7.664027248171309203, -32.00000000000000000 ) ) ;
#15714 = ORIENTED_EDGE ( 'NONE', *, *, #15674, .F. ) ;
#15715 = CARTESIAN_POINT ( 'NONE',  ( -2.000000000000001776, 0.000000000000000000, -7.800000000000000711 ) ) ;
#15716 = FACE_OUTER_BOUND ( 'NONE', #16576, .T. ) ;
#15717 = ORIENTED_EDGE ( 'NONE', *, *, #13684, .T. ) ;
#15718 = TOROIDAL_SURFACE ( 'NONE', #7064, -32.79058411375427795, 40.00000000000000711 ) ;
#15719 = VECTOR ( 'NONE', #10696, 1000.000000000000000 ) ;
#15720 = VECTOR ( 'NONE', #733, 1000.000000000000000 ) ;
#15721 = CARTESIAN_POINT ( 'NONE',  ( 9.312499995903225525, 3.350375938067097437, -4.611396867937201272 ) ) ;
#15722 = ORIENTED_EDGE ( 'NONE', *, *, #453, .T. ) ;
#15723 = CARTESIAN_POINT ( 'NONE',  ( 2.718184749312774429, -25.22524549359948409, -2.576941577947671647 ) ) ;
#15724 = CARTESIAN_POINT ( 'NONE',  ( -1.493657965219446160, 5.574407415329178939, -14.81249999590322375 ) ) ;
#15725 = FACE_OUTER_BOUND ( 'NONE', #5721, .T. ) ;
#15726 = AXIS2_PLACEMENT_3D ( 'NONE', #13781, #10586, #4475 ) ;
#15727 = ORIENTED_EDGE ( 'NONE', *, *, #3337, .F. ) ;
#15728 = DIRECTION ( 'NONE',  ( -0.000000000000000000, 0.000000000000000000, 1.000000000000000000 ) ) ;
#15729 = ORIENTED_EDGE ( 'NONE', *, *, #7702, .T. ) ;
#15730 = CARTESIAN_POINT ( 'NONE',  ( 0.000000000000000000, 0.000000000000000000, -6.000000000000005329 ) ) ;
#15731 = ORIENTED_EDGE ( 'NONE', *, *, #8779, .T. ) ;
#15732 = DIRECTION ( 'NONE',  ( -0.000000000000000000, -0.000000000000000000, 1.000000000000000000 ) ) ;
#15733 = ADVANCED_FACE ( 'NONE', ( #12825 ), #9098, .F. ) ;
#15734 = CARTESIAN_POINT ( 'NONE',  ( 1.394999999999999574, -12.52377138324241734, 25.12109765559649688 ) ) ;
#15735 = B_SPLINE_CURVE_WITH_KNOTS ( 'NONE', 3,
 ( #5052, #17464, #15964, #4958 ),
 .UNSPECIFIED., .F., .F.,
 ( 4, 4 ),
 ( 0.000000000000000000, 0.001126652051248517271 ),
 .UNSPECIFIED. ) ;
#15736 = CARTESIAN_POINT ( 'NONE',  ( -4.500000000000000000, 0.000000000000000000, -35.00000000000000000 ) ) ;
#15737 = AXIS2_PLACEMENT_3D ( 'NONE', #289, #9599, #494 ) ;
#15738 = AXIS2_PLACEMENT_3D ( 'NONE', #2657, #13462, #4369 ) ;
#15739 = CARTESIAN_POINT ( 'NONE',  ( 2.444050593750020095, 4.233219804643871598, -6.843749997951615427 ) ) ;
#15740 = VERTEX_POINT ( 'NONE', #13608 ) ;
#15741 = AXIS2_PLACEMENT_3D ( 'NONE', #16698, #2980, #9094 ) ;
#15742 = FACE_OUTER_BOUND ( 'NONE', #19359, .T. ) ;
#15743 = DIRECTION ( 'NONE',  ( 0.000000000000000000, 0.000000000000000000, 1.000000000000000000 ) ) ;
#15744 = ORIENTED_EDGE ( 'NONE', *, *, #8, .F. ) ;
#15745 = EDGE_CURVE ( 'NONE', #3868, #14825, #4173, .T. ) ;
#15746 = VECTOR ( 'NONE', #15580, 1000.000000000000000 ) ;
#15747 = FACE_OUTER_BOUND ( 'NONE', #11641, .T. ) ;
#15748 = CARTESIAN_POINT ( 'NONE',  ( -4.465502636338010589, 1.988169868018623720, -14.46874999795161720 ) ) ;
#15749 = CARTESIAN_POINT ( 'NONE',  ( -4.781284448697201483, -1.016293382781378485, -12.46874999795161543 ) ) ;
#15750 = EDGE_LOOP ( 'NONE', ( #11616, #11843, #7647, #16543 ) ) ;
#15751 = AXIS2_PLACEMENT_3D ( 'NONE', #17988, #10680, #16584 ) ;
#15752 = PLANE ( 'NONE',  #19771 ) ;
#15753 = EDGE_CURVE ( 'NONE', #12919, #9230, #4305, .T. ) ;
#15754 = DIRECTION ( 'NONE',  ( -1.000000000000000000, -0.000000000000000000, -0.000000000000000000 ) ) ;
#15755 = AXIS2_PLACEMENT_3D ( 'NONE', #7420, #6027, #13438 ) ;
#15756 = ORIENTED_EDGE ( 'NONE', *, *, #7081, .T. ) ;
#15757 = CARTESIAN_POINT ( 'NONE',  ( 13.00000000000000533, 0.5958122406256767256, -5.668774803599153422 ) ) ;
#15758 = ORIENTED_EDGE ( 'NONE', *, *, #8757, .T. ) ;
#15759 = VECTOR ( 'NONE', #13851, 1000.000000000000000 ) ;
#15760 = APPLICATION_PROTOCOL_DEFINITION ( 'draft international standard', 'automotive_design', 1998, #8430 ) ;
#15761 = CARTESIAN_POINT ( 'NONE',  ( 7.843749997951614539, 3.270778111535313837, 3.632567103900546712 ) ) ;
#15762 = CARTESIAN_POINT ( 'NONE',  ( 12.34374999795161543, 1.773574444220725299, 4.620319390059829168 ) ) ;
#15763 = VERTEX_POINT ( 'NONE', #1206 ) ;
#15764 =( BOUNDED_CURVE ( )  B_SPLINE_CURVE ( 2, ( #10487, #3066, #169, #2765, #6161, #7458, #7354, #19770, #1474, #12280, #13578, #8881, #18378, #14982, #15181, #4377, #4670 ),
 .UNSPECIFIED., .F., .F. ) 
 B_SPLINE_CURVE_WITH_KNOTS ( ( 3, 2, 2, 2, 2, 2, 2, 2, 3 ),
 ( 0.000000000000000000, 0.05000000000000000971, 0.1000000000000000194, 0.1499999999999999944, 0.2000000000000000389, 0.2500000000000000000, 0.2999999999999999889, 0.3499999999999999223, 0.4000000000000000777 ),
 .UNSPECIFIED. ) 
 CURVE ( )  GEOMETRIC_REPRESENTATION_ITEM ( )  RATIONAL_B_SPLINE_CURVE ( ( 1.000000000000000000, 0.9876883405951377704, 1.000000000000000000, 0.9876883405951377704, 1.000000000000000000, 0.9876883405951377704, 1.000000000000000000, 0.9876883405951377704, 1.000000000000000000, 0.9876883405951377704, 1.000000000000000000, 0.9876883405951377704, 1.000000000000000000, 0.9876883405951377704, 1.000000000000000000, 0.9876883405951377704, 1.000000000000000000 ) ) 
 REPRESENTATION_ITEM ( '' )  );
#15765 = ORIENTED_EDGE ( 'NONE', *, *, #11877, .F. ) ;
#15766 = DIRECTION ( 'NONE',  ( -1.000000000000000000, -1.224646799147353207E-16, 0.000000000000000000 ) ) ;
#15767 = PLANE ( 'NONE',  #16869 ) ;
#15768 = ORIENTED_EDGE ( 'NONE', *, *, #5115, .T. ) ;
#15769 = CIRCLE ( 'NONE', #7422, 24.12539914357697768 ) ;
#15770 = EDGE_CURVE ( 'NONE', #16827, #677, #18542, .T. ) ;
#15771 = CARTESIAN_POINT ( 'NONE',  ( -1.280903732194386802, 4.780397808154273065, -14.34374999795161543 ) ) ;
#15772 = ORIENTED_EDGE ( 'NONE', *, *, #18739, .F. ) ;
#15773 = CIRCLE ( 'NONE', #10352, 1.000000000000003553 ) ;
#15774 = CYLINDRICAL_SURFACE ( 'NONE', #7094, 1.000000000000002665 ) ;
#15775 = CARTESIAN_POINT ( 'NONE',  ( 0.07181525696555239591, 24.78695292654921545, 5.344212458769448837 ) ) ;
#15776 =( GEOMETRIC_REPRESENTATION_CONTEXT ( 3 ) GLOBAL_UNCERTAINTY_ASSIGNED_CONTEXT ( ( #16204 ) ) GLOBAL_UNIT_ASSIGNED_CONTEXT ( ( #6673, #8086, #7986 ) ) REPRESENTATION_CONTEXT ( 'NONE', 'WORKASPACE' ) );
#15777 = ORIENTED_EDGE ( 'NONE', *, *, #6277, .T. ) ;
#15778 = DIRECTION ( 'NONE',  ( 0.000000000000000000, 0.000000000000000000, 1.000000000000000000 ) ) ;
#15779 = DIRECTION ( 'NONE',  ( -1.000000000000000000, -0.000000000000000000, -0.000000000000000000 ) ) ;
#15780 = VERTEX_POINT ( 'NONE', #16515 ) ;
#15781 = EDGE_CURVE ( 'NONE', #4160, #8143, #12476, .T. ) ;
#15782 = VERTEX_POINT ( 'NONE', #11810 ) ;
#15783 = CARTESIAN_POINT ( 'NONE',  ( -2.318398865532001363, 5.207209108562852684, -13.00000000000000533 ) ) ;
#15784 = DIRECTION ( 'NONE',  ( 9.559896011775280412E-17, 0.7806247497997995666, -0.6250000000000001110 ) ) ;
#15785 = EDGE_CURVE ( 'NONE', #4579, #5395, #8704, .T. ) ;
#15786 = CARTESIAN_POINT ( 'NONE',  ( -3.143139765844555900, 4.840010801796527318, -13.81249999590322552 ) ) ;
#15787 = ORIENTED_EDGE ( 'NONE', *, *, #17169, .F. ) ;
#15788 = DIRECTION ( 'NONE',  ( -0.4999999999999978351, 0.7499999999999990008, 0.4330127018922234616 ) ) ;
#15789 = ADVANCED_FACE ( 'NONE', ( #16416 ), #9009, .F. ) ;
#15790 = DIRECTION ( 'NONE',  ( -1.000000000000000000, -0.000000000000000000, -0.000000000000000000 ) ) ;
#15791 = ORIENTED_EDGE ( 'NONE', *, *, #1103, .T. ) ;
#15792 = CARTESIAN_POINT ( 'NONE',  ( 2.765633920072236407, 2.336989772644613161, -24.63872515616080250 ) ) ;
#15793 = CARTESIAN_POINT ( 'NONE',  ( -11.00000000000000355, 4.898587196589412829E-16, 0.000000000000000000 ) ) ;
#15794 = AXIS2_PLACEMENT_3D ( 'NONE', #11516, #5595, #5692 ) ;
#15795 = LINE ( 'NONE', #12694, #4860 ) ;
#15796 = DIRECTION ( 'NONE',  ( -1.000000000000000000, -0.000000000000000000, 0.000000000000000000 ) ) ;
#15797 = CARTESIAN_POINT ( 'NONE',  ( -1.761396867937238042, -5.421022142882365280, -12.00000000000000533 ) ) ;
#15798 = CARTESIAN_POINT ( 'NONE',  ( 8.312499995903225525, 3.814044456245473835, 4.235925505221166176 ) ) ;
#15799 = FACE_OUTER_BOUND ( 'NONE', #17449, .T. ) ;
#15800 = CARTESIAN_POINT ( 'NONE',  ( 6.626241948324199882, -16.73597674598852691, 32.00000000000000000 ) ) ;
#15801 = ORIENTED_EDGE ( 'NONE', *, *, #18017, .T. ) ;
#15802 = FACE_OUTER_BOUND ( 'NONE', #5634, .T. ) ;
#15803 = CIRCLE ( 'NONE', #11004, 4.400000000000000355 ) ;
#15804 = DIRECTION ( 'NONE',  ( 1.000000000000000000, 0.000000000000000000, 0.000000000000000000 ) ) ;
#15805 = CARTESIAN_POINT ( 'NONE',  ( 4.235925505221166176, 3.814044456245473835, -8.312499995903225525 ) ) ;
#15806 = CARTESIAN_POINT ( 'NONE',  ( 13.00000000000000178, -3.789407127742538517, 3.087705756618167374 ) ) ;
#15807 = CARTESIAN_POINT ( 'NONE',  ( -90.00000000000000000, 0.000000000000000000, 0.000000000000000000 ) ) ;
#15808 = ORIENTED_EDGE ( 'NONE', *, *, #7498, .T. ) ;
#15809 = CARTESIAN_POINT ( 'NONE',  ( 0.000000000000000000, 23.48180575137729775, 5.535312321042836103 ) ) ;
#15810 = MANIFOLD_SOLID_BREP ( 'Base-Revolve', #18000 ) ;
#15811 = CARTESIAN_POINT ( 'NONE',  ( 2.765633920072238627, -21.30679549418621832, -12.59161484032935618 ) ) ;
#15812 = ORIENTED_EDGE ( 'NONE', *, *, #15770, .F. ) ;
#15813 = CIRCLE ( 'NONE', #4624, 0.9999999999999974465 ) ;
#15814 = EDGE_CURVE ( 'NONE', #5327, #12828, #664, .T. ) ;
#15815 = CARTESIAN_POINT ( 'NONE',  ( 13.81249999590322552, -5.142044285764733935, -2.620002426024580000 ) ) ;
#15816 = ADVANCED_FACE ( 'NONE', ( #11912 ), #3204, .T. ) ;
#15817 = CYLINDRICAL_SURFACE ( 'NONE', #9474, 9.000000000000001776 ) ;
#15818 = ORIENTED_EDGE ( 'NONE', *, *, #2581, .F. ) ;
#15819 = CIRCLE ( 'NONE', #2690, 0.9999999999999974465 ) ;
#15820 = ADVANCED_FACE ( 'NONE', ( #6186 ), #4604, .T. ) ;
#15821 = CARTESIAN_POINT ( 'NONE',  ( 13.00000000000000178, -0.7793280607714923036, -4.825575716215948496 ) ) ;
#15822 = CARTESIAN_POINT ( 'NONE',  ( 91.50000000000000000, 4.401380596135586802E-16, -3.593999999999999861 ) ) ;
#15823 = VERTEX_POINT ( 'NONE', #101 ) ;
#15824 = CARTESIAN_POINT ( 'NONE',  ( 2.789999999999999147, 12.59161484032912171, 21.30679549418635688 ) ) ;
#15825 = CARTESIAN_POINT ( 'NONE',  ( 5.476417968967387750, 17.43449690031536292, -32.00000000000000000 ) ) ;
#15826 = FACE_BOUND ( 'NONE', #18300, .T. ) ;
#15827 = EDGE_LOOP ( 'NONE', ( #15765, #248, #4741, #11721, #13055, #3627 ) ) ;
#15828 = LINE ( 'NONE', #11225, #16619 ) ;
#15829 = VERTEX_POINT ( 'NONE', #10710 ) ;
#15830 = EDGE_CURVE ( 'NONE', #562, #13990, #7341, .T. ) ;
#15831 = CARTESIAN_POINT ( 'NONE',  ( 2.031033491000350466, -24.80232951178386713, 12.05173163741713083 ) ) ;
#15832 = ORIENTED_EDGE ( 'NONE', *, *, #18708, .T. ) ;
#15833 = EDGE_CURVE ( 'NONE', #14379, #1977, #9410, .T. ) ;
#15834 = DIRECTION ( 'NONE',  ( 0.000000000000000000, 0.000000000000000000, -1.000000000000000000 ) ) ;
#15835 = CARTESIAN_POINT ( 'NONE',  ( 1.899999999999999023, 1.010590785124388747E-15, 8.239200000000002078 ) ) ;
#15836 = DIRECTION ( 'NONE',  ( 0.000000000000000000, 0.000000000000000000, 1.000000000000000000 ) ) ;
#15837 = CONICAL_SURFACE ( 'NONE', #7176, 6.735000000000022524, 0.3653297453805129935 ) ;
#15838 = CARTESIAN_POINT ( 'NONE',  ( 4.942249507334556036, -0.2590123213421313686, -10.34374999795161543 ) ) ;
#15839 = CIRCLE ( 'NONE', #17759, 1.000000000000004441 ) ;
#15840 = ORIENTED_EDGE ( 'NONE', *, *, #17523, .T. ) ;
#15841 = FACE_BOUND ( 'NONE', #16852, .T. ) ;
#15842 = CARTESIAN_POINT ( 'NONE',  ( 2.790000000000000480, 9.514945144208736494, 22.37986894186676423 ) ) ;
#15843 = ORIENTED_EDGE ( 'NONE', *, *, #2322, .F. ) ;
#15844 = CARTESIAN_POINT ( 'NONE',  ( -4.611396867937224364, -3.350375938067065906, -14.00000000000000533 ) ) ;
#15845 = EDGE_CURVE ( 'NONE', #16305, #16734, #12810, .T. ) ;
#15846 = CYLINDRICAL_SURFACE ( 'NONE', #17933, 4.000000000000000000 ) ;
#15847 = CARTESIAN_POINT ( 'NONE',  ( -2.695436003842760719, -4.150607464521772094, -9.968749997951615427 ) ) ;
#15848 = ORIENTED_EDGE ( 'NONE', *, *, #7878, .T. ) ;
#15849 = AXIS2_PLACEMENT_3D ( 'NONE', #18164, #12750, #4947 ) ;
#15850 = DIRECTION ( 'NONE',  ( -1.000000000000000000, 0.000000000000000000, 0.000000000000000000 ) ) ;
#15851 = CARTESIAN_POINT ( 'NONE',  ( 4.648860486681943627, -1.510506337161893864, -7.468749997951615427 ) ) ;
#15852 = DIRECTION ( 'NONE',  ( -0.000000000000000000, -0.000000000000000000, 1.000000000000000000 ) ) ;
#15853 = AXIS2_PLACEMENT_3D ( 'NONE', #1717, #16928, #13817 ) ;
#15854 = VERTEX_POINT ( 'NONE', #14095 ) ;
#15855 = CARTESIAN_POINT ( 'NONE',  ( 2.647025296875021638, 4.584782303107579615, -6.234374998975811266 ) ) ;
#15856 = ADVANCED_FACE ( 'NONE', ( #3096 ), #15373, .T. ) ;
#15857 = EDGE_LOOP ( 'NONE', ( #8213, #11819, #1577, #18322, #5868 ) ) ;
#15858 = CONTEXT_DEPENDENT_SHAPE_REPRESENTATION ( #3860, #13376 ) ;
#15859 = SURFACE_SIDE_STYLE ('',( #2342 ) ) ;
#15860 = ADVANCED_FACE ( 'NONE', ( #11001 ), #7793, .T. ) ;
#15861 = CARTESIAN_POINT ( 'NONE',  ( 7.843749997951614539, 4.781284448697194378, -1.016293382781411125 ) ) ;
#15862 = ORIENTED_EDGE ( 'NONE', *, *, #4183, .F. ) ;
#15863 = EDGE_LOOP ( 'NONE', ( #3143, #9487, #17060, #9175, #10756, #18189 ) ) ;
#15864 = CARTESIAN_POINT ( 'NONE',  ( 0.000000000000000000, 0.000000000000000000, -32.00000000000000000 ) ) ;
#15865 = CARTESIAN_POINT ( 'NONE',  ( 7.812499995903224637, -0.9027913098498966393, 5.699999999999994849 ) ) ;
#15866 = CARTESIAN_POINT ( 'NONE',  ( -2.000000000000000000, -5.000000000000001776, 37.99999999999999289 ) ) ;
#15867 = ORIENTED_EDGE ( 'NONE', *, *, #10864, .T. ) ;
#15868 = ADVANCED_FACE ( 'NONE', ( #10807 ), #4901, .T. ) ;
#15869 = CIRCLE ( 'NONE', #11382, 5.400000000000000355 ) ;
#15870 = DIRECTION ( 'NONE',  ( -0.000000000000000000, 0.000000000000000000, -1.000000000000000000 ) ) ;
#15871 = ORIENTED_EDGE ( 'NONE', *, *, #13623, .T. ) ;
#15872 = DIRECTION ( 'NONE',  ( -1.000000000000000000, 0.000000000000000000, 0.000000000000000000 ) ) ;
#15873 = LINE ( 'NONE', #13165, #7409 ) ;
#15874 =( BOUNDED_CURVE ( )  B_SPLINE_CURVE ( 2, ( #19197, #16119, #995, #7072, #2394, #5303, #2680, #2582, #8509 ),
 .UNSPECIFIED., .F., .F. ) 
 B_SPLINE_CURVE_WITH_KNOTS ( ( 3, 2, 2, 2, 3 ),
 ( 0.000000000000000000, 0.04999999999999999584, 0.09999999999999999167, 0.1499999999999999944, 0.1666819079834116757 ),
 .UNSPECIFIED. ) 
 CURVE ( )  GEOMETRIC_REPRESENTATION_ITEM ( )  RATIONAL_B_SPLINE_CURVE ( ( 1.000000000000000000, 0.9876883405951377704, 1.000000000000000000, 0.9876883405951377704, 1.000000000000000000, 0.9876883405951377704, 1.000000000000000000, 0.9958923606136996787, 0.9945256517182512468 ) ) 
 REPRESENTATION_ITEM ( '' )  );
#15875 = CARTESIAN_POINT ( 'NONE',  ( 2.031033467310410234, -12.98167595241039329, 24.32849926382746020 ) ) ;
#15876 = MANIFOLD_SOLID_BREP ( 'Boss-Extrude3', #7416 ) ;
#15877 = ORIENTED_EDGE ( 'NONE', *, *, #13238, .T. ) ;
#15878 =( REPRESENTATION_RELATIONSHIP ('NONE','NONE', #18211, #7967 ) REPRESENTATION_RELATIONSHIP_WITH_TRANSFORMATION ( #13050 )SHAPE_REPRESENTATION_RELATIONSHIP( ) );
#15879 = CARTESIAN_POINT ( 'NONE',  ( 0.07181525480391401373, -21.92234060054336098, -12.74223776959224708 ) ) ;
#15880 = LINE ( 'NONE', #6848, #14783 ) ;
#15881 = ADVANCED_FACE ( 'NONE', ( #14006 ), #17275, .T. ) ;
#15882 = CIRCLE ( 'NONE', #19697, 1.000000000000000888 ) ;
#15883 = ORIENTED_EDGE ( 'NONE', *, *, #1710, .T. ) ;
#15884 = ORIENTED_EDGE ( 'NONE', *, *, #11779, .T. ) ;
#15885 = CARTESIAN_POINT ( 'NONE',  ( -4.936344801571268093, 2.850000000000057820, -11.00000000000000711 ) ) ;
#15886 = CARTESIAN_POINT ( 'NONE',  ( 12.00000000000000178, 1.469576158976824144E-15, 29.00000000000000355 ) ) ;
#15887 = CARTESIAN_POINT ( 'NONE',  ( 1.039999999999997593, 0.000000000000000000, 0.000000000000000000 ) ) ;
#15888 = VERTEX_POINT ( 'NONE', #12608 ) ;
#15889 = CARTESIAN_POINT ( 'NONE',  ( -4.476417968967385974, 17.43449690031536292, 35.00000000000000000 ) ) ;
#15890 = CARTESIAN_POINT ( 'NONE',  ( 9.343749997951615427, -1.280903732194386579, -4.780397808154273953 ) ) ;
#15891 = AXIS2_PLACEMENT_3D ( 'NONE', #17944, #7514, #16447 ) ;
#15892 = ORIENTED_EDGE ( 'NONE', *, *, #3667, .T. ) ;
#15893 = PLANE ( 'NONE',  #17744 ) ;
#15894 = CIRCLE ( 'NONE', #5330, 1.000000000000004441 ) ;
#15895 = EDGE_CURVE ( 'NONE', #5399, #12952, #12410, .T. ) ;
#15896 = DIRECTION ( 'NONE',  ( 1.000000000000000000, 0.000000000000000000, 0.000000000000000000 ) ) ;
#15897 = CARTESIAN_POINT ( 'NONE',  ( -17.68117051311639898, -3.372863662543042818, -35.00000000000000000 ) ) ;
#15898 = CYLINDRICAL_SURFACE ( 'NONE', #5558, 0.9999999999999974465 ) ;
#15899 = FACE_OUTER_BOUND ( 'NONE', #1147, .T. ) ;
#15900 = CARTESIAN_POINT ( 'NONE',  ( 8.812499995903225525, 3.143139765844590983, 4.840010801796506001 ) ) ;
#15901 = CARTESIAN_POINT ( 'NONE',  ( 0.000000000000000000, 1.991882183130315953, 24.04302995059967074 ) ) ;
#15902 = EDGE_CURVE ( 'NONE', #1763, #2041, #3299, .T. ) ;
#15903 = DIRECTION ( 'NONE',  ( -1.000000000000000000, -0.000000000000000000, -0.000000000000000000 ) ) ;
#15904 = ORIENTED_EDGE ( 'NONE', *, *, #9573, .T. ) ;
#15905 = CARTESIAN_POINT ( 'NONE',  ( 0.000000000000000000, -9.324097380959319281, -22.25075486061748009 ) ) ;
#15906 = TOROIDAL_SURFACE ( 'NONE', #14301, 24.12539914357697768, 8.000000000000000000 ) ;
#15907 = CARTESIAN_POINT ( 'NONE',  ( 5.207209108562838473, 2.318398865532038666, -9.312499995903225525 ) ) ;
#15908 = CIRCLE ( 'NONE', #18132, 7.937500000000000000 ) ;
#15909 = CARTESIAN_POINT ( 'NONE',  ( 7.843749997951614539, -4.781284448697200595, 1.016293382781377819 ) ) ;
#15910 = ORIENTED_EDGE ( 'NONE', *, *, #19070, .T. ) ;
#15911 = B_SPLINE_CURVE_WITH_KNOTS ( 'NONE', 3,
 ( #4082, #6668, #17398, #3682 ),
 .UNSPECIFIED., .F., .F.,
 ( 4, 4 ),
 ( 0.005258110598983608240, 0.005948376585272727862 ),
 .UNSPECIFIED. ) ;
#15912 = CARTESIAN_POINT ( 'NONE',  ( -4.888101187500000222, 0.000000000000000000, -6.843749997951615427 ) ) ;
#15913 = VERTEX_POINT ( 'NONE', #17298 ) ;
#15914 = CARTESIAN_POINT ( 'NONE',  ( 12.84374999795161543, -4.648860486681943627, -1.510506337161893642 ) ) ;
#15915 = DIRECTION ( 'NONE',  ( -1.000000000000000000, -0.000000000000000000, -0.000000000000000000 ) ) ;
#15916 = ORIENTED_EDGE ( 'NONE', *, *, #7599, .F. ) ;
#15917 = LINE ( 'NONE', #8413, #14545 ) ;
#15918 = CARTESIAN_POINT ( 'NONE',  ( 2.444050593750020095, 4.233219804643871598, -6.468749997951615427 ) ) ;
#15919 = AXIS2_PLACEMENT_3D ( 'NONE', #19285, #17500, #2288 ) ;
#15920 = AXIS2_PLACEMENT_3D ( 'NONE', #15713, #3307, #6583 ) ;
#15921 = DIRECTION ( 'NONE',  ( -0.4999999999999979461, -0.7500000000000021094, 0.4330127018922180770 ) ) ;
#15922 = LINE ( 'NONE', #9930, #17059 ) ;
#15923 = ORIENTED_EDGE ( 'NONE', *, *, #11893, .F. ) ;
#15924 = DIRECTION ( 'NONE',  ( 1.000000000000000000, 0.000000000000000000, 0.000000000000000000 ) ) ;
#15925 = FACE_OUTER_BOUND ( 'NONE', #11010, .T. ) ;
#15926 = ADVANCED_FACE ( 'NONE', ( #14510 ), #13358, .F. ) ;
#15927 = ORIENTED_EDGE ( 'NONE', *, *, #17570, .T. ) ;
#15928 = CARTESIAN_POINT ( 'NONE',  ( 12.46874999795161543, -4.648860486681943627, -1.510506337161893642 ) ) ;
#15929 = VERTEX_POINT ( 'NONE', #12999 ) ;
#15930 = EDGE_CURVE ( 'NONE', #8517, #9243, #9911, .T. ) ;
#15931 = LINE ( 'NONE', #17529, #9512 ) ;
#15932 = ORIENTED_EDGE ( 'NONE', *, *, #3560, .F. ) ;
#15933 = CARTESIAN_POINT ( 'NONE',  ( 7.937500000000000000, -4.582717761692665981, -6.527800000000000047 ) ) ;
#15934 = CARTESIAN_POINT ( 'NONE',  ( -5.700000000000001066, 0.000000000000000000, -7.312499995903225525 ) ) ;
#15935 = PRODUCT ( 'DRIVER', 'DRIVER', '', ( #4655 ) ) ;
#15936 = CYLINDRICAL_SURFACE ( 'NONE', #16360, 2.524999999999995914 ) ;
#15937 = AXIS2_PLACEMENT_3D ( 'NONE', #14870, #10569, #1163 ) ;
#15938 = CARTESIAN_POINT ( 'NONE',  ( 1.280903732194421663, -4.780397808154265960, -14.34374999795161365 ) ) ;
#15939 = ORIENTED_EDGE ( 'NONE', *, *, #9442, .F. ) ;
#15940 = CARTESIAN_POINT ( 'NONE',  ( -16.28688694438836038, -7.664027248171298545, -32.00000000000000000 ) ) ;
#15941 = EDGE_CURVE ( 'NONE', #11964, #19760, #5750, .T. ) ;
#15942 = CARTESIAN_POINT ( 'NONE',  ( 1.749999999999998002, 0.000000000000000000, 0.000000000000000000 ) ) ;
#15943 = EDGE_LOOP ( 'NONE', ( #3642, #8000 ) ) ;
#15944 = FACE_OUTER_BOUND ( 'NONE', #16159, .T. ) ;
#15946 = EDGE_CURVE ( 'NONE', #15913, #15001, #17587, .T. ) ;
#15945 = EDGE_CURVE ( 'NONE', #15354, #4315, #13122, .T. ) ;
#15947 = FACE_OUTER_BOUND ( 'NONE', #12324, .T. ) ;
#15948 = DIRECTION ( 'NONE',  ( 0.000000000000000000, -1.000000000000000000, 0.000000000000000000 ) ) ;
#15949 = CIRCLE ( 'NONE', #5398, 2.524999999999998135 ) ;
#15950 = ORIENTED_EDGE ( 'NONE', *, *, #861, .T. ) ;
#15951 = CARTESIAN_POINT ( 'NONE',  ( 22.00000000000000355, 2.694222958124177204E-15, -32.00000000000000000 ) ) ;
#15952 = CARTESIAN_POINT ( 'NONE',  ( 2.299999999999996270, 0.000000000000000000, 0.000000000000000000 ) ) ;
#15953 = CARTESIAN_POINT ( 'NONE',  ( 1.869199999999999973, 1.009010990753487416E-15, 8.239200000000002078 ) ) ;
#15954 = ORIENTED_EDGE ( 'NONE', *, *, #6737, .F. ) ;
#15955 = CARTESIAN_POINT ( 'NONE',  ( 0.000000000000000000, -18.28042085475266632, -15.74360496233403239 ) ) ;
#15956 = ORIENTED_EDGE ( 'NONE', *, *, #5764, .T. ) ;
#15957 = CONTEXT_DEPENDENT_SHAPE_REPRESENTATION ( #10015, #7130 ) ;
#15958 = DIRECTION ( 'NONE',  ( 0.000000000000000000, 0.000000000000000000, 1.000000000000000000 ) ) ;
#15959 = CARTESIAN_POINT ( 'NONE',  ( 0.000000000000000000, 0.000000000000000000, -33.00000000000000000 ) ) ;
#15960 = ORIENTED_EDGE ( 'NONE', *, *, #12764, .F. ) ;
#15961 = ORIENTED_EDGE ( 'NONE', *, *, #9879, .F. ) ;
#15962 = CARTESIAN_POINT ( 'NONE',  ( 0.000000000000000000, -5.535312321042547445, -23.48180575137738302 ) ) ;
#15963 = DIRECTION ( 'NONE',  ( 0.000000000000000000, 0.000000000000000000, 1.000000000000000000 ) ) ;
#15964 = CARTESIAN_POINT ( 'NONE',  ( 12.99999999999969980, -1.390454305316078276, -5.264438301130803133 ) ) ;
#15965 = VERTEX_POINT ( 'NONE', #11495 ) ;
#15966 = AXIS2_PLACEMENT_3D ( 'NONE', #9782, #6346, #3366 ) ;
#15967 = PLANE ( 'NONE',  #13497 ) ;
#15968 = CIRCLE ( 'NONE', #8938, 28.06981291497571007 ) ;
#15969 = VERTEX_POINT ( 'NONE', #15996 ) ;
#15970 = DIRECTION ( 'NONE',  ( -1.000000000000000000, 0.000000000000000000, 0.000000000000000000 ) ) ;
#15971 = CARTESIAN_POINT ( 'NONE',  ( 1.749999999999998002, 20.02152543075374069, -19.67366047555509212 ) ) ;
#15972 = FACE_OUTER_BOUND ( 'NONE', #5119, .T. ) ;
#15973 = ORIENTED_EDGE ( 'NONE', *, *, #8983, .T. ) ;
#15974 = DIRECTION ( 'NONE',  ( 1.000000000000000000, 0.000000000000000000, 0.000000000000000000 ) ) ;
#15975 = CARTESIAN_POINT ( 'NONE',  ( 4.233219804643887585, 2.444050593749990785, -11.46874999795161543 ) ) ;
#15976 = ORIENTED_EDGE ( 'NONE', *, *, #2785, .F. ) ;
#15977 = ORIENTED_EDGE ( 'NONE', *, *, #9173, .T. ) ;
#15978 = CARTESIAN_POINT ( 'NONE',  ( 2.790000000000000924, 0.000000000000000000, 4.000000000000000000 ) ) ;
#15979 = AXIS2_PLACEMENT_3D ( 'NONE', #10540, #6020, #19436 ) ;
#15980 = CIRCLE ( 'NONE', #12793, 2.524999999999996358 ) ;
#15981 = CARTESIAN_POINT ( 'NONE',  ( 2.790000000000000036, -15.96500990068111214, -18.34424029220128816 ) ) ;
#15982 = DIRECTION ( 'NONE',  ( -0.000000000000000000, -0.000000000000000000, 1.000000000000000000 ) ) ;
#15983 = ORIENTED_EDGE ( 'NONE', *, *, #18978, .T. ) ;
#15984 = CARTESIAN_POINT ( 'NONE',  ( 7.468749997951615427, -3.270778111535287191, -3.632567103900569361 ) ) ;
#15985 = CARTESIAN_POINT ( 'NONE',  ( 13.00000000000000533, -4.021726346896400628, 2.778353902928540453 ) ) ;
#15986 = ORIENTED_EDGE ( 'NONE', *, *, #9883, .T. ) ;
#15987 = CARTESIAN_POINT ( 'NONE',  ( 2.789999999999999147, 0.000000000000000000, 0.000000000000000000 ) ) ;
#15988 = EDGE_CURVE ( 'NONE', #15854, #4661, #8975, .T. ) ;
#15989 = CIRCLE ( 'NONE', #16952, 1.000000000000004441 ) ;
#15990 = STYLED_ITEM ( 'NONE', ( #17971 ), #16005 ) ;
#15991 = DIRECTION ( 'NONE',  ( 0.000000000000000000, 0.000000000000000000, 1.000000000000000000 ) ) ;
#15992 = CARTESIAN_POINT ( 'NONE',  ( -36.00000000000000000, 1.999999999999999112, 2.000000000000000000 ) ) ;
#15993 = CARTESIAN_POINT ( 'NONE',  ( 2.789999999999999147, -24.34211360614305875, 7.909232158574721616 ) ) ;
#15994 = CYLINDRICAL_SURFACE ( 'NONE', #9167, 1.000000000000004441 ) ;
#15995 = DIRECTION ( 'NONE',  ( 1.000000000000000000, 0.000000000000000000, 0.000000000000000000 ) ) ;
#15996 = CARTESIAN_POINT ( 'NONE',  ( 3.255998204157476206, -17.85806462366060288, 35.00000000000000000 ) ) ;
#15997 = ORIENTED_EDGE ( 'NONE', *, *, #6477, .T. ) ;
#15998 = DIRECTION ( 'NONE',  ( -1.000000000000000000, -0.000000000000000000, -0.000000000000000000 ) ) ;
#15999 = FACE_BOUND ( 'NONE', #14488, .T. ) ;
#16000 = PRODUCT_DEFINITION_CONTEXT ( 'detailed design', #5712, 'design' ) ;
#16001 = CARTESIAN_POINT ( 'NONE',  ( 0.000000000000000000, 0.000000000000000000, 12.00000000000000000 ) ) ;
#16002 = CARTESIAN_POINT ( 'NONE',  ( 8.468749997951615427, -4.861323657744403448, -0.5109457054262123155 ) ) ;
#16003 = EDGE_CURVE ( 'NONE', #18935, #15675, #14867, .T. ) ;
#16004 = DIRECTION ( 'NONE',  ( 0.000000000000000000, 0.000000000000000000, 1.000000000000000000 ) ) ;
#16005 = MANIFOLD_SOLID_BREP ( 'Boss-Extrude1', #8751 ) ;
#16006 = AXIS2_PLACEMENT_3D ( 'NONE', #8310, #8415, #8699 ) ;
#16007 = CARTESIAN_POINT ( 'NONE',  ( -2.000000000000001776, 3.478305785123968707, -3.241971077674649315 ) ) ;
#16008 = ORIENTED_EDGE ( 'NONE', *, *, #17901, .T. ) ;
#16009 = CARTESIAN_POINT ( 'NONE',  ( 16.28688694438835327, -7.664027248171309203, -32.00000000000000000 ) ) ;
#16010 = DIRECTION ( 'NONE',  ( 0.000000000000000000, 0.000000000000000000, -1.000000000000000000 ) ) ;
#16011 = VERTEX_POINT ( 'NONE', #5185 ) ;
#16012 = SURFACE_SIDE_STYLE ('',( #6691 ) ) ;
#16013 = EDGE_CURVE ( 'NONE', #9137, #6839, #15968, .T. ) ;
#16014 = FACE_BOUND ( 'NONE', #3359, .T. ) ;
#16015 = CARTESIAN_POINT ( 'NONE',  ( 5.500000000000005329, -4.015688387708123076E-15, 32.79058411375427795 ) ) ;
#16016 = CARTESIAN_POINT ( 'NONE',  ( 8.000000000000000000, 1.999999999999997335, 41.99999999999999289 ) ) ;
#16017 = EDGE_LOOP ( 'NONE', ( #4378, #18285 ) ) ;
#16018 = AXIS2_PLACEMENT_3D ( 'NONE', #1545, #16955, #19651 ) ;
#16019 = CARTESIAN_POINT ( 'NONE',  ( 0.02436607992776151574, -18.55949924794880346, -16.37294372382878649 ) ) ;
#16020 =( NAMED_UNIT ( * ) SI_UNIT ( $, .STERADIAN. ) SOLID_ANGLE_UNIT ( ) );
#16021 = CARTESIAN_POINT ( 'NONE',  ( -8.671566133830875600, 15.77352024078954429, 35.00000000000000000 ) ) ;
#16022 = AXIS2_PLACEMENT_3D ( 'NONE', #9141, #16747, #6021 ) ;
#16023 = ORIENTED_EDGE ( 'NONE', *, *, #13545, .T. ) ;
#16024 = DIRECTION ( 'NONE',  ( -0.000000000000000000, -0.000000000000000000, 1.000000000000000000 ) ) ;
#16025 = ORIENTED_EDGE ( 'NONE', *, *, #6826, .T. ) ;
#16026 = CARTESIAN_POINT ( 'NONE',  ( -16.68117051311640253, -3.372863662543042818, -32.00000000000000000 ) ) ;
#16027 = EDGE_LOOP ( 'NONE', ( #6256, #6231, #17127, #14793, #13229, #11915 ) ) ;
#16028 = CARTESIAN_POINT ( 'NONE',  ( -3.968750000000004441, 6.874076642538978987, 0.000000000000000000 ) ) ;
#16029 = CARTESIAN_POINT ( 'NONE',  ( 1.749999999999998002, 25.12109765559671004, -12.52377138324198391 ) ) ;
#16030 = EDGE_CURVE ( 'NONE', #1752, #18366, #5722, .T. ) ;
#16031 = DIRECTION ( 'NONE',  ( 0.000000000000000000, 0.000000000000000000, 1.000000000000000000 ) ) ;
#16032 = LINE ( 'NONE', #16229, #3133 ) ;
#16033 = ORIENTED_EDGE ( 'NONE', *, *, #12376, .F. ) ;
#16034 = CARTESIAN_POINT ( 'NONE',  ( 2.718184745196085661, 12.74223776959200727, 21.92234060054350309 ) ) ;
#16035 = CARTESIAN_POINT ( 'NONE',  ( 3.255998204157476206, -17.85806462366060288, -32.00000000000000000 ) ) ;
#16036 = ADVANCED_FACE ( 'NONE', ( #9162 ), #5947, .T. ) ;
#16037 = AXIS2_PLACEMENT_3D ( 'NONE', #9952, #11535, #7105 ) ;
#16038 = EDGE_LOOP ( 'NONE', ( #2048, #15220, #14360, #17198 ) ) ;
#16039 = AXIS2_PLACEMENT_3D ( 'NONE', #12297, #3280, #7973 ) ;
#16040 = AXIS2_PLACEMENT_3D ( 'NONE', #13813, #12417, #4806 ) ;
#16041 = EDGE_CURVE ( 'NONE', #14247, #16782, #10665, .T. ) ;
#16042 = MANIFOLD_SOLID_BREP ( 'Base-Revolve', #11594 ) ;
#16043 = CARTESIAN_POINT ( 'NONE',  ( 89.62500000000000000, 4.898587196589412829E-16, -4.000000000000000000 ) ) ;
#16044 = CARTESIAN_POINT ( 'NONE',  ( -0.7741991708319226895, -4.888101187499994893, -12.34374999795161543 ) ) ;
#16045 = ORIENTED_EDGE ( 'NONE', *, *, #14193, .F. ) ;
#16046 = CARTESIAN_POINT ( 'NONE',  ( 16.96448111170888851, 1.130229351527639148, -32.00000000000000000 ) ) ;
#16047 = B_SPLINE_CURVE_WITH_KNOTS ( 'NONE', 3,
 ( #14583, #872, #6952, #2067 ),
 .UNSPECIFIED., .F., .F.,
 ( 4, 4 ),
 ( 0.005258105385878691744, 0.005948373736081389272 ),
 .UNSPECIFIED. ) ;
#16048 = CARTESIAN_POINT ( 'NONE',  ( -2.873153789725852558, -3.954556930911842016, -13.46874999795161543 ) ) ;
#16049 = FACE_BOUND ( 'NONE', #6146, .T. ) ;
#16050 = ORIENTED_EDGE ( 'NONE', *, *, #16502, .T. ) ;
#16051 = EDGE_CURVE ( 'NONE', #17411, #11356, #18517, .T. ) ;
#16052 = DIRECTION ( 'NONE',  ( 0.000000000000000000, 0.000000000000000000, 1.000000000000000000 ) ) ;
#16053 = CIRCLE ( 'NONE', #2302, 1.000000000000002665 ) ;
#16054 = ORIENTED_EDGE ( 'NONE', *, *, #19212, .F. ) ;
#16055 = AXIS2_PLACEMENT_3D ( 'NONE', #10283, #2460, #8668 ) ;
#16056 = DIRECTION ( 'NONE',  ( 1.000000000000000000, 0.000000000000000000, 0.000000000000000000 ) ) ;
#16057 = CYLINDRICAL_SURFACE ( 'NONE', #7310, 4.000000000000000000 ) ;
#16058 = AXIS2_PLACEMENT_3D ( 'NONE', #18003, #5580, #16206 ) ;
#16059 = CARTESIAN_POINT ( 'NONE',  ( 16.96448111170888851, 1.130229351527639148, -32.00000000000000000 ) ) ;
#16060 = ORIENTED_EDGE ( 'NONE', *, *, #7174, .F. ) ;
#16061 = CARTESIAN_POINT ( 'NONE',  ( 0.8291131470075020493, -24.44424927289185590, 12.96989951879399072 ) ) ;
#16062 = CARTESIAN_POINT ( 'NONE',  ( 7.500000000000005329, 3.143139765844590983, 4.840010801796506001 ) ) ;
#16063 = CARTESIAN_POINT ( 'NONE',  ( -0.5958122406255597081, 5.668774803599165857, -14.00000000000000533 ) ) ;
#16064 = EDGE_CURVE ( 'NONE', #12845, #5267, #15233, .T. ) ;
#16065 = EDGE_LOOP ( 'NONE', ( #19638, #17719, #5337, #14241 ) ) ;
#16066 = EDGE_CURVE ( 'NONE', #14722, #17321, #16278, .T. ) ;
#16067 = B_SPLINE_CURVE_WITH_KNOTS ( 'NONE', 3,
 ( #13371, #2561, #5567, #19373 ),
 .UNSPECIFIED., .F., .F.,
 ( 4, 4 ),
 ( 0.005258214619651953650, 0.005948481662034169060 ),
 .UNSPECIFIED. ) ;
#16068 = CARTESIAN_POINT ( 'NONE',  ( 0.02436607992776064838, 5.391175441198615914, 24.15498966839965078 ) ) ;
#16069 = B_SPLINE_CURVE_WITH_KNOTS ( 'NONE', 3,
 ( #10932, #7916, #14229, #3223, #15831, #3426 ),
 .UNSPECIFIED., .F., .F.,
 ( 4, 2, 4 ),
 ( 2.586195665736120714E-07, 0.001878649493629689022, 0.003757040367692804708 ),
 .UNSPECIFIED. ) ;
#16070 = AXIS2_PLACEMENT_3D ( 'NONE', #12083, #13677, #18185 ) ;
#16071 = VERTEX_POINT ( 'NONE', #1257 ) ;
#16072 = VECTOR ( 'NONE', #5460, 1000.000000000000000 ) ;
#16073 = CLOSED_SHELL ( 'NONE', ( #14980, #18184, #2196, #10927, #17393, #6912, #5873, #11431, #16758, #12359, #6104, #8094, #10057, #9227, #19361, #3470, #5041, #18372, #4922, #18712, #8063, #2695, #14365, #4016, #17929, #16180, #10317, #4490, #16811, #11849, #9373, #14428, #13474, #476, #2711, #5300, #2754, #8223, #3463, #10489, #7287, #12969, #14844, #5030 ) ) ;
#16074 = CYLINDRICAL_SURFACE ( 'NONE', #16602, 2.524999999999995914 ) ;
#16075 = EDGE_CURVE ( 'NONE', #12580, #6991, #10895, .T. ) ;
#16076 = CIRCLE ( 'NONE', #17342, 1.000000000000004441 ) ;
#16077 = DIRECTION ( 'NONE',  ( -1.000000000000000000, 0.000000000000000000, 0.000000000000000000 ) ) ;
#16078 = EDGE_LOOP ( 'NONE', ( #7135, #11024, #2805, #12138, #18895, #7542 ) ) ;
#16079 = DIRECTION ( 'NONE',  ( 1.000000000000000000, 0.000000000000000000, 0.000000000000000000 ) ) ;
#16080 = DIRECTION ( 'NONE',  ( 0.000000000000000000, 0.000000000000000000, 1.000000000000000000 ) ) ;
#16081 = DIRECTION ( 'NONE',  ( 0.000000000000000000, 0.000000000000000000, -1.000000000000000000 ) ) ;
#16082 = ORIENTED_EDGE ( 'NONE', *, *, #8120, .T. ) ;
#16083 = ORIENTED_EDGE ( 'NONE', *, *, #10518, .F. ) ;
#16084 = CARTESIAN_POINT ( 'NONE',  ( -4.780397808154273953, -1.280903732194386579, -8.968749997951611874 ) ) ;
#16085 = EDGE_CURVE ( 'NONE', #18433, #608, #311, .T. ) ;
#16086 = AXIS2_PLACEMENT_3D ( 'NONE', #17862, #8955, #16466 ) ;
#16087 = ADVANCED_FACE ( 'NONE', ( #7333 ), #1580, .T. ) ;
#16088 = FACE_OUTER_BOUND ( 'NONE', #2909, .T. ) ;
#16089 = TOROIDAL_SURFACE ( 'NONE', #11606, 6.000000000000000000, 1.199999999999999956 ) ;
#16090 = VERTEX_POINT ( 'NONE', #4360 ) ;
#16091 = CARTESIAN_POINT ( 'NONE',  ( 9.843749997951615427, -0.5109457054261099529, -4.861323657744413218 ) ) ;
#16092 = VECTOR ( 'NONE', #1895, 1000.000000000000000 ) ;
#16093 = CARTESIAN_POINT ( 'NONE',  ( 10.81249999590322375, 0.3020334839683282424, -5.763142191869152775 ) ) ;
#16094 = ORIENTED_EDGE ( 'NONE', *, *, #15225, .T. ) ;
#16095 = LINE ( 'NONE', #2177, #13273 ) ;
#16096 = PRESENTATION_LAYER_ASSIGNMENT (  '', '', ( #15452 ) ) ;
#16097 = CARTESIAN_POINT ( 'NONE',  ( 1.749999999999998002, -12.52377138324206030, -25.12109765559667096 ) ) ;
#16098 = EDGE_CURVE ( 'NONE', #10667, #10763, #16571, .T. ) ;
#16099 = CARTESIAN_POINT ( 'NONE',  ( 18.96448111170889206, 1.130229351527639370, -32.00000000000000000 ) ) ;
#16100 = CARTESIAN_POINT ( 'NONE',  ( -13.86923836996420967, -11.47363181547641275, -32.00000000000000000 ) ) ;
#16101 = PRODUCT_DEFINITION_SHAPE ( 'NONE', 'NONE',  #2339 ) ;
#16102 = DIRECTION ( 'NONE',  ( 1.000000000000000000, 0.000000000000000000, 0.000000000000000000 ) ) ;
#16103 = CARTESIAN_POINT ( 'NONE',  ( -4.476417968967385974, 17.43449690031536292, 32.00000000000000000 ) ) ;
#16104 = CIRCLE ( 'NONE', #16746, 1.000000000000004441 ) ;
#16105 =( NAMED_UNIT ( * ) SI_UNIT ( $, .STERADIAN. ) SOLID_ANGLE_UNIT ( ) );
#16106 = ORIENTED_EDGE ( 'NONE', *, *, #10806, .F. ) ;
#16107 = CARTESIAN_POINT ( 'NONE',  ( 12.00000000000000000, 0.000000000000000000, 0.000000000000000000 ) ) ;
#16108 = CARTESIAN_POINT ( 'NONE',  ( -20.63749999999999574, 8.786840783882257924E-16, 7.174999999999998934 ) ) ;
#16109 = CARTESIAN_POINT ( 'NONE',  ( 2.318398865532038666, -5.207209108562836697, -14.31249999590322552 ) ) ;
#16110 = EDGE_CURVE ( 'NONE', #18594, #2162, #14258, .T. ) ;
#16111 = CARTESIAN_POINT ( 'NONE',  ( 7.968749997951616315, -4.942249507334558700, 0.2590123213420631454 ) ) ;
#16112 = DIRECTION ( 'NONE',  ( 1.000000000000000000, 0.000000000000000000, 0.000000000000000000 ) ) ;
#16113 =( GEOMETRIC_REPRESENTATION_CONTEXT ( 3 ) GLOBAL_UNCERTAINTY_ASSIGNED_CONTEXT ( ( #13385 ) ) GLOBAL_UNIT_ASSIGNED_CONTEXT ( ( #3786, #7159, #5381 ) ) REPRESENTATION_CONTEXT ( 'NONE', 'WORKASPACE' ) );
#16114 = AXIS2_PLACEMENT_3D ( 'NONE', #8679, #14787, #11490 ) ;
#16115 = CARTESIAN_POINT ( 'NONE',  ( -5.699999999999999289, 0.9027913098498568933, -7.812499995903224637 ) ) ;
#16116 = ORIENTED_EDGE ( 'NONE', *, *, #8754, .T. ) ;
#16117 = CARTESIAN_POINT ( 'NONE',  ( 14.84374999795161543, -2.873153789725797935, -3.954556930911881096 ) ) ;
#16118 =( BOUNDED_SURFACE ( )  B_SPLINE_SURFACE ( 1, 2, ( 
 ( #2544, #11566, #5361, #17477, #12975, #17378, #13169, #1061, #5158, #9888, #15975, #9980, #14487, #19067, #868, #8764, #9161 ),
 ( #5743, #15268, #13267, #1256, #16570, #2746, #4158, #16366, #19357, #1458, #6043, #5650, #4456, #13560, #15063, #18170, #1358 ) ),
 .UNSPECIFIED., .F., .F., .F. ) 
 B_SPLINE_SURFACE_WITH_KNOTS ( ( 2, 2 ),
 ( 3, 2, 2, 2, 2, 2, 2, 2, 3 ),
 ( 0.000000000000000000, 1.000000000000000000 ),
 ( 0.000000000000000000, 0.05000000000000000278, 0.1000000000000000056, 0.1499999999999999944, 0.2000000000000000111, 0.2500000000000000000, 0.2999999999999999889, 0.3499999999999999778, 0.4000000000000000222 ),
 .UNSPECIFIED. ) 
 GEOMETRIC_REPRESENTATION_ITEM ( )  RATIONAL_B_SPLINE_SURFACE ( (
 ( 1.000000000000000000, 0.9876883405951377704, 1.000000000000000000, 0.9876883405951377704, 1.000000000000000000, 0.9876883405951377704, 1.000000000000000000, 0.9876883405951377704, 1.000000000000000000, 0.9876883405951377704, 1.000000000000000000, 0.9876883405951377704, 1.000000000000000000, 0.9876883405951377704, 1.000000000000000000, 0.9876883405951377704, 1.000000000000000000),
 ( 1.000000000000000000, 0.9876883405951377704, 1.000000000000000000, 0.9876883405951377704, 1.000000000000000000, 0.9876883405951377704, 1.000000000000000000, 0.9876883405951377704, 1.000000000000000000, 0.9876883405951377704, 1.000000000000000000, 0.9876883405951377704, 1.000000000000000000, 0.9876883405951377704, 1.000000000000000000, 0.9876883405951377704, 1.000000000000000000) ) ) 
 REPRESENTATION_ITEM ( '' )  SURFACE ( )  );
#16119 = CARTESIAN_POINT ( 'NONE',  ( 3.631840208645826795, 4.484949146646356688, -7.812499995903224637 ) ) ;
#16120 = EDGE_LOOP ( 'NONE', ( #7439, #7984, #12461, #12500 ) ) ;
#16121 = DIRECTION ( 'NONE',  ( 0.000000000000000000, 0.000000000000000000, -1.000000000000000000 ) ) ;
#16122 = EDGE_CURVE ( 'NONE', #9700, #9124, #7002, .T. ) ;
#16123 = AXIS2_PLACEMENT_3D ( 'NONE', #976, #18992, #17590 ) ;
#16124 = CARTESIAN_POINT ( 'NONE',  ( 1.799999999999999600, 9.797174393178825657E-16, 8.000000000000000000 ) ) ;
#16125 = DIRECTION ( 'NONE',  ( 0.000000000000000000, 0.000000000000000000, -1.000000000000000000 ) ) ;
#16126 = LINE ( 'NONE', #11419, #769 ) ;
#16127 = ORIENTED_EDGE ( 'NONE', *, *, #4044, .T. ) ;
#16128 = CIRCLE ( 'NONE', #1422, 5.700000000000001954 ) ;
#16129 = B_SPLINE_CURVE_WITH_KNOTS ( 'NONE', 3,
 ( #12242, #10639, #9239, #12043 ),
 .UNSPECIFIED., .F., .F.,
 ( 4, 4 ),
 ( 2.135345996700793610E-07, 0.0006888010880211471818 ),
 .UNSPECIFIED. ) ;
#16130 = FACE_OUTER_BOUND ( 'NONE', #8220, .T. ) ;
#16131 = SHAPE_REPRESENTATION_RELATIONSHIP ( 'NONE' , 'NONE' ,  #13463, #12355 ) ;
#16132 = DIRECTION ( 'NONE',  ( 1.000000000000000000, -0.000000000000000000, -0.000000000000000000 ) ) ;
#16133 = CARTESIAN_POINT ( 'NONE',  ( 3.968750000000000000, 0.000000000000000000, -0.5557897334539606549 ) ) ;
#16134 = ORIENTED_EDGE ( 'NONE', *, *, #14812, .F. ) ;
#16135 = DIRECTION ( 'NONE',  ( 0.000000000000000000, 0.000000000000000000, -1.000000000000000000 ) ) ;
#16136 = ORIENTED_EDGE ( 'NONE', *, *, #17741, .T. ) ;
#16137 = CARTESIAN_POINT ( 'NONE',  ( 0.000000000000000000, -1.991882183130475603, 24.04302995059966719 ) ) ;
#16138 = ADVANCED_FACE ( 'NONE', ( #7844 ), #17065, .T. ) ;
#16139 = AXIS2_PLACEMENT_3D ( 'NONE', #8116, #9738, #723 ) ;
#16140 = DIRECTION ( 'NONE',  ( 1.000000000000000000, 6.419766481290786633E-33, -0.000000000000000000 ) ) ;
#16141 = FACE_OUTER_BOUND ( 'NONE', #1260, .T. ) ;
#16142 = DIRECTION ( 'NONE',  ( 1.000000000000000000, 0.000000000000000000, 0.000000000000000000 ) ) ;
#16143 = ORIENTED_EDGE ( 'NONE', *, *, #1665, .F. ) ;
#16144 = DIRECTION ( 'NONE',  ( -1.224646799147353207E-16, 1.000000000000000000, 0.000000000000000000 ) ) ;
#16145 = LINE ( 'NONE', #11821, #13937 ) ;
#16146 = ORIENTED_EDGE ( 'NONE', *, *, #12769, .T. ) ;
#16147 = ADVANCED_FACE ( 'NONE', ( #560 ), #17269, .F. ) ;
#16148 = CARTESIAN_POINT ( 'NONE',  ( 0.6492350739116989899, 8.790599478695050095, -0.4925372136696584136 ) ) ;
#16149 = EDGE_CURVE ( 'NONE', #9454, #11016, #10851, .T. ) ;
#16150 = DIRECTION ( 'NONE',  ( 0.000000000000000000, 0.000000000000000000, 1.000000000000000000 ) ) ;
#16151 = ADVANCED_FACE ( 'NONE', ( #14052 ), #18554, .F. ) ;
#16152 = ORIENTED_EDGE ( 'NONE', *, *, #858, .T. ) ;
#16153 = CARTESIAN_POINT ( 'NONE',  ( 2.789999999999999147, 23.48180575137730131, 5.535312321042802353 ) ) ;
#16154 = FACE_OUTER_BOUND ( 'NONE', #3756, .T. ) ;
#16155 = FACE_BOUND ( 'NONE', #14550, .T. ) ;
#16156 = ORIENTED_EDGE ( 'NONE', *, *, #8918, .F. ) ;
#16157 = LINE ( 'NONE', #13245, #3977 ) ;
#16158 = CIRCLE ( 'NONE', #7826, 1.000000000000003109 ) ;
#16159 = EDGE_LOOP ( 'NONE', ( #11002, #7712, #4786, #9411 ) ) ;
#16160 = ITEM_DEFINED_TRANSFORMATION ( 'NONE', 'NONE', #18183,  #16724 ) ;
#16161 =( NAMED_UNIT ( * ) PLANE_ANGLE_UNIT ( ) SI_UNIT ( $, .RADIAN. ) );
#16162 = DIRECTION ( 'NONE',  ( -1.000000000000000000, -0.000000000000000000, -0.000000000000000000 ) ) ;
#16163 = ADVANCED_FACE ( 'NONE', ( #11055 ), #3545, .T. ) ;
#16164 = DIRECTION ( 'NONE',  ( -0.000000000000000000, -0.000000000000000000, 1.000000000000000000 ) ) ;
#16165 = ORIENTED_EDGE ( 'NONE', *, *, #783, .F. ) ;
#16166 = CARTESIAN_POINT ( 'NONE',  ( -39.64101615137792578, 82.80384757729314060, 37.99999999999999289 ) ) ;
#16167 = DIRECTION ( 'NONE',  ( 1.000000000000000000, 0.000000000000000000, 0.000000000000000000 ) ) ;
#16168 = DIRECTION ( 'NONE',  ( 0.000000000000000000, 0.000000000000000000, -1.000000000000000000 ) ) ;
#16169 = EDGE_LOOP ( 'NONE', ( #446, #15567 ) ) ;
#16170 = B_SPLINE_CURVE_WITH_KNOTS ( 'NONE', 3,
 ( #4570, #8781, #8879, #13576 ),
 .UNSPECIFIED., .F., .F.,
 ( 4, 4 ),
 ( 3.059063720760159520E-07, 0.0006888942284914070097 ),
 .UNSPECIFIED. ) ;
#16171 = CARTESIAN_POINT ( 'NONE',  ( 0.000000000000000000, 5.700000000000001954, -6.000000000000005329 ) ) ;
#16172 = VECTOR ( 'NONE', #2826, 1000.000000000000000 ) ;
#16173 = EDGE_LOOP ( 'NONE', ( #5454, #2173 ) ) ;
#16174 = FACE_OUTER_BOUND ( 'NONE', #12140, .T. ) ;
#16175 = CARTESIAN_POINT ( 'NONE',  ( 8.000000000000005329, -3.350375938067129855, 4.611396867937178179 ) ) ;
#16176 = ORIENTED_EDGE ( 'NONE', *, *, #14735, .F. ) ;
#16177 = CARTESIAN_POINT ( 'NONE',  ( -2.695436003842674566, 4.150607464521828938, -13.34374999795161365 ) ) ;
#16178 = MANIFOLD_SOLID_BREP ( 'Extrude-Thin1', #17382 ) ;
#16179 = CARTESIAN_POINT ( 'NONE',  ( 0.000000000000000000, 0.000000000000000000, 0.000000000000000000 ) ) ;
#16180 = ADVANCED_FACE ( 'NONE', ( #13145 ), #8039, .T. ) ;
#16181 = ORIENTED_EDGE ( 'NONE', *, *, #14856, .F. ) ;
#16182 = EDGE_LOOP ( 'NONE', ( #14829, #2862, #13765, #7474 ) ) ;
#16183 = EDGE_CURVE ( 'NONE', #15059, #241, #5829, .T. ) ;
#16184 = CARTESIAN_POINT ( 'NONE',  ( -2.444050593750049849, -4.233219804643852946, -6.468749997951615427 ) ) ;
#16185 = TOROIDAL_SURFACE ( 'NONE', #14901, 24.12539914357697413, 8.000000000000000000 ) ;
#16186 = DIRECTION ( 'NONE',  ( 0.000000000000000000, 0.000000000000000000, -1.000000000000000000 ) ) ;
#16187 = AXIS2_PLACEMENT_3D ( 'NONE', #2102, #8304, #5097 ) ;
#16188 = DIRECTION ( 'NONE',  ( 0.000000000000000000, 0.000000000000000000, -1.000000000000000000 ) ) ;
#16189 = ORIENTED_EDGE ( 'NONE', *, *, #4441, .T. ) ;
#16190 = CARTESIAN_POINT ( 'NONE',  ( -2.255998204157477538, -17.85806462366060288, -35.00000000000000000 ) ) ;
#16191 = EDGE_CURVE ( 'NONE', #15404, #13931, #5533, .T. ) ;
#16192 = CARTESIAN_POINT ( 'NONE',  ( 13.00000000000000000, 3.840809689103004576, -4.211671987713725862 ) ) ;
#16193 = VERTEX_POINT ( 'NONE', #1140 ) ;
#16194 = LINE ( 'NONE', #8489, #817 ) ;
#16195 = ADVANCED_FACE ( 'NONE', ( #19148 ), #4140, .F. ) ;
#16196 = LINE ( 'NONE', #3781, #10296 ) ;
#16197 = LINE ( 'NONE', #19278, #6827 ) ;
#16198 = DIRECTION ( 'NONE',  ( -1.000000000000000000, 0.000000000000000000, 0.000000000000000000 ) ) ;
#16199 = CARTESIAN_POINT ( 'NONE',  ( -5.209999999999999964, 0.000000000000000000, 0.000000000000000000 ) ) ;
#16200 = CARTESIAN_POINT ( 'NONE',  ( 2.789679245949062913, -20.70663861606260525, -12.51925356660783528 ) ) ;
#16201 = ORIENTED_EDGE ( 'NONE', *, *, #7528, .T. ) ;
#16202 = CARTESIAN_POINT ( 'NONE',  ( 10.31249999590322552, 5.207209108562820710, 2.318398865532073749 ) ) ;
#16203 = DIRECTION ( 'NONE',  ( 1.000000000000000000, 0.000000000000000000, 0.000000000000000000 ) ) ;
#16204 = UNCERTAINTY_MEASURE_WITH_UNIT (LENGTH_MEASURE( 1.000000000000000082E-05 ), #6673, 'distance_accuracy_value', 'NONE');
#16205 = CARTESIAN_POINT ( 'NONE',  ( 5.668774803599163192, 0.5958122406255991210, -10.31249999590322552 ) ) ;
#16206 = DIRECTION ( 'NONE',  ( 0.000000000000000000, -0.8660254037844398178, 0.4999999999999978351 ) ) ;
#16207 = CIRCLE ( 'NONE', #17799, 8.000000000000000000 ) ;
#16208 = CARTESIAN_POINT ( 'NONE',  ( -1.761396867937200739, 5.421022142882375938, -11.31249999590322375 ) ) ;
#16209 = VERTEX_POINT ( 'NONE', #17747 ) ;
#16210 = CARTESIAN_POINT ( 'NONE',  ( -10.99900000000000233, -4.200000000000000178, 0.000000000000000000 ) ) ;
#16211 = ADVANCED_FACE ( 'NONE', ( #755 ), #7213, .F. ) ;
#16212 = CARTESIAN_POINT ( 'NONE',  ( 0.000000000000000000, -5.000000000000001776, 37.99999999999999289 ) ) ;
#16213 = VERTEX_POINT ( 'NONE', #3844 ) ;
#16214 = DIRECTION ( 'NONE',  ( -1.000000000000000000, 0.000000000000000000, 0.000000000000000000 ) ) ;
#16215 = PLANE ( 'NONE',  #11845 ) ;
#16216 = DIRECTION ( 'NONE',  ( -1.000000000000000000, -0.000000000000000000, -0.000000000000000000 ) ) ;
#16217 = CARTESIAN_POINT ( 'NONE',  ( -1.886022603841296830, 0.000000000000000000, -6.735000000000022524 ) ) ;
#16218 = ORIENTED_EDGE ( 'NONE', *, *, #18190, .F. ) ;
#16219 = CIRCLE ( 'NONE', #6934, 4.200000000000000178 ) ;
#16220 = CARTESIAN_POINT ( 'NONE',  ( -16.68117051311640253, -3.372863662543042818, 32.00000000000000000 ) ) ;
#16221 = CARTESIAN_POINT ( 'NONE',  ( 2.789999999999999147, 0.000000000000000000, 0.000000000000000000 ) ) ;
#16222 = DIRECTION ( 'NONE',  ( -1.000000000000000000, -0.000000000000000000, -0.000000000000000000 ) ) ;
#16223 = ORIENTED_EDGE ( 'NONE', *, *, #16355, .F. ) ;
#16224 = CARTESIAN_POINT ( 'NONE',  ( 2.789999999999999147, 5.535312321042718864, 23.48180575137732262 ) ) ;
#16225 = ORIENTED_EDGE ( 'NONE', *, *, #18082, .T. ) ;
#16226 = APPLICATION_CONTEXT ( 'automotive_design' ) ;
#16227 = DIRECTION ( 'NONE',  ( -1.000000000000000000, 0.000000000000000000, 0.000000000000000000 ) ) ;
#16228 = CARTESIAN_POINT ( 'NONE',  ( 13.00000000000000000, 5.567819778318904511, 1.220402768007685657 ) ) ;
#16229 = CARTESIAN_POINT ( 'NONE',  ( 2.999999999999998224, 3.950217066951266176, -3.681818181818181213 ) ) ;
#16230 = ORIENTED_EDGE ( 'NONE', *, *, #74, .F. ) ;
#16231 = CARTESIAN_POINT ( 'NONE',  ( 2.444050593749960587, -4.233219804643904460, -6.843749997951615427 ) ) ;
#16232 = CARTESIAN_POINT ( 'NONE',  ( 13.00000000000000000, -3.840809689102975710, 4.211671987713753396 ) ) ;
#16233 = CIRCLE ( 'NONE', #17829, 24.12539914357697768 ) ;
#16234 = ORIENTED_EDGE ( 'NONE', *, *, #3261, .F. ) ;
#16235 = CIRCLE ( 'NONE', #6629, 0.9999999999999974465 ) ;
#16236 = EDGE_CURVE ( 'NONE', #9061, #488, #7638, .T. ) ;
#16237 = DIRECTION ( 'NONE',  ( 1.000000000000000000, 0.000000000000000000, 0.000000000000000000 ) ) ;
#16238 = FACE_OUTER_BOUND ( 'NONE', #16880, .T. ) ;
#16239 = VERTEX_POINT ( 'NONE', #3748 ) ;
#16240 = CYLINDRICAL_SURFACE ( 'NONE', #4919, 4.400000000000000355 ) ;
#16241 = B_SPLINE_CURVE_WITH_KNOTS ( 'NONE', 3,
 ( #9528, #18816, #17028, #13925 ),
 .UNSPECIFIED., .F., .F.,
 ( 4, 4 ),
 ( 0.003263275852154340524, 0.003756984793530001795 ),
 .UNSPECIFIED. ) ;
#16242 = DIRECTION ( 'NONE',  ( 0.8660254037844330455, -0.5000000000000098810, 0.000000000000000000 ) ) ;
#16243 = DIRECTION ( 'NONE',  ( 0.000000000000000000, 0.000000000000000000, 1.000000000000000000 ) ) ;
#16244 = ORIENTED_EDGE ( 'NONE', *, *, #9651, .F. ) ;
#16245 = DIRECTION ( 'NONE',  ( -1.000000000000000000, 0.000000000000000000, 0.000000000000000000 ) ) ;
#16247 = DIRECTION ( 'NONE',  ( -1.000000000000000000, -0.000000000000000000, -0.000000000000000000 ) ) ;
#16246 = AXIS2_PLACEMENT_3D ( 'NONE', #9188, #4679, #13783 ) ;
#16248 = EDGE_LOOP ( 'NONE', ( #14675, #10711, #8408, #12968 ) ) ;
#16249 = CARTESIAN_POINT ( 'NONE',  ( -1.000000000000001998, 18.00000000000000355, -32.00000000000000000 ) ) ;
#16250 = DIRECTION ( 'NONE',  ( -1.000000000000000000, -0.000000000000000000, -0.000000000000000000 ) ) ;
#16251 = EDGE_LOOP ( 'NONE', ( #8467, #578, #13239, #19396 ) ) ;
#16252 = DIRECTION ( 'NONE',  ( 1.000000000000000000, 0.000000000000000000, 0.000000000000000000 ) ) ;
#16253 = CARTESIAN_POINT ( 'NONE',  ( 9.312499995903225525, -3.350375938067129855, 4.611396867937178179 ) ) ;
#16254 = LINE ( 'NONE', #17952, #3438 ) ;
#16255 = ORIENTED_EDGE ( 'NONE', *, *, #2835, .F. ) ;
#16256 = ADVANCED_FACE ( 'NONE', ( #11642 ), #5627, .F. ) ;
#16257 = B_SPLINE_CURVE_WITH_KNOTS ( 'NONE', 3,
 ( #2484, #14899, #14704, #11896 ),
 .UNSPECIFIED., .F., .F.,
 ( 4, 4 ),
 ( 0.005258139959819239928, 0.005948405594583421920 ),
 .UNSPECIFIED. ) ;
#16258 = B_SPLINE_CURVE_WITH_KNOTS ( 'NONE', 3,
 ( #12868, #19062, #13065, #7033 ),
 .UNSPECIFIED., .F., .F.,
 ( 4, 4 ),
 ( 0.000000000000000000, 0.001125480700308659253 ),
 .UNSPECIFIED. ) ;
#16259 = DIRECTION ( 'NONE',  ( -1.000000000000000000, 0.000000000000000000, 0.000000000000000000 ) ) ;
#16260 = PRODUCT_DEFINITION_SHAPE ( 'NONE', 'NONE',  #19795 ) ;
#16261 = AXIS2_PLACEMENT_3D ( 'NONE', #9166, #2953, #15273 ) ;
#16262 = ORIENTED_EDGE ( 'NONE', *, *, #15171, .F. ) ;
#16263 = ADVANCED_FACE ( 'NONE', ( #17845 ), #16057, .F. ) ;
#16264 = B_SPLINE_CURVE_WITH_KNOTS ( 'NONE', 3,
 ( #17313, #17511, #8410, #7171, #11413, #3800 ),
 .UNSPECIFIED., .F., .F.,
 ( 4, 2, 4 ),
 ( 4.462636731830560059E-07, 0.001879885066974964830, 0.003759323870276746679 ),
 .UNSPECIFIED. ) ;
#16265 = FACE_OUTER_BOUND ( 'NONE', #19402, .T. ) ;
#16266 = PRODUCT_DEFINITION_FORMATION_WITH_SPECIFIED_SOURCE ( 'ANY', '', #12896, .NOT_KNOWN. ) ;
#16267 = LINE ( 'NONE', #3960, #5200 ) ;
#16268 = ORIENTED_EDGE ( 'NONE', *, *, #286, .F. ) ;
#16269 = CARTESIAN_POINT ( 'NONE',  ( -4.150607464521828938, -2.695436003842674566, -8.343749997951611874 ) ) ;
#16270 = B_SPLINE_CURVE_WITH_KNOTS ( 'NONE', 3,
 ( #398, #14008, #14203, #508 ),
 .UNSPECIFIED., .F., .F.,
 ( 4, 4 ),
 ( 1.981826382900813409E-07, 0.0006887856082032186092 ),
 .UNSPECIFIED. ) ;
#16271 = VERTEX_POINT ( 'NONE', #5340 ) ;
#16272 = ORIENTED_EDGE ( 'NONE', *, *, #7104, .F. ) ;
#16273 = CARTESIAN_POINT ( 'NONE',  ( -15.19790265903627180, 9.644882309621941374, 32.00000000000000000 ) ) ;
#16274 = CIRCLE ( 'NONE', #10208, 24.12539914357697768 ) ;
#16275 = DIRECTION ( 'NONE',  ( 1.000000000000000000, 0.000000000000000000, 0.000000000000000000 ) ) ;
#16276 = ORIENTED_EDGE ( 'NONE', *, *, #10417, .T. ) ;
#16277 = EDGE_CURVE ( 'NONE', #18135, #639, #17566, .T. ) ;
#16278 = CIRCLE ( 'NONE', #14045, 1.000000000000002665 ) ;
#16279 = CARTESIAN_POINT ( 'NONE',  ( 7.937500000000000000, 0.000000000000000000, 0.000000000000000000 ) ) ;
#16280 = EDGE_LOOP ( 'NONE', ( #9772, #19550, #12834, #2310, #4826, #6652, #212, #9529 ) ) ;
#16281 = CARTESIAN_POINT ( 'NONE',  ( 5.700000000000002842, 2.725425358843983450E-16, -9.332722423957255486 ) ) ;
#16282 = CARTESIAN_POINT ( 'NONE',  ( 13.00000000000000178, -3.947414994554141021, 2.883678330714922300 ) ) ;
#16283 = ADVANCED_FACE ( 'NONE', ( #11546 ), #11491, .T. ) ;
#16284 = ORIENTED_EDGE ( 'NONE', *, *, #2179, .F. ) ;
#16285 = CARTESIAN_POINT ( 'NONE',  ( -15.00000000000000355, 1.224646799147353454E-16, 0.000000000000000000 ) ) ;
#16286 = EDGE_CURVE ( 'NONE', #7772, #3249, #3943, .T. ) ;
#16287 = DIRECTION ( 'NONE',  ( -0.000000000000000000, 1.000000000000000000, 1.224646799147353207E-16 ) ) ;
#16288 = CARTESIAN_POINT ( 'NONE',  ( 5.645569974854462103, 5.905964178674214082, -0.1296323192022580117 ) ) ;
#16289 = CARTESIAN_POINT ( 'NONE',  ( 9.843749997951615427, -4.465502636338009701, -1.988169868018624609 ) ) ;
#16290 = AXIS2_PLACEMENT_3D ( 'NONE', #8323, #730, #11523 ) ;
#16291 = CARTESIAN_POINT ( 'NONE',  ( -11.00000000000000355, 3.278623949159159778, 2.625000000000000888 ) ) ;
#16292 = DIRECTION ( 'NONE',  ( 0.000000000000000000, 0.000000000000000000, 1.000000000000000000 ) ) ;
#16293 = VERTEX_POINT ( 'NONE', #7621 ) ;
#16294 = ADVANCED_FACE ( 'NONE', ( #5822 ), #4431, .F. ) ;
#16295 = DIRECTION ( 'NONE',  ( 0.000000000000000000, 0.000000000000000000, 1.000000000000000000 ) ) ;
#16296 = DIRECTION ( 'NONE',  ( -1.000000000000000000, 0.000000000000000000, -0.000000000000000000 ) ) ;
#16297 = CARTESIAN_POINT ( 'NONE',  ( -3.814044456245444081, 4.235925505221192822, -12.00000000000000533 ) ) ;
#16298 = CYLINDRICAL_SURFACE ( 'NONE', #13823, 6.735000000000022524 ) ;
#16299 = CARTESIAN_POINT ( 'NONE',  ( 1.761396867937200073, 5.421022142882376826, -13.31249999590322730 ) ) ;
#16300 = EDGE_CURVE ( 'NONE', #15416, #19054, #3186, .T. ) ;
#16301 = ORIENTED_EDGE ( 'NONE', *, *, #5857, .F. ) ;
#16302 = CARTESIAN_POINT ( 'NONE',  ( -39.64101615137763446, 12.80384757729311573, 37.99999999999999289 ) ) ;
#16303 = CARTESIAN_POINT ( 'NONE',  ( 0.000000000000000000, 4.999999999999998224, 37.99999999999999289 ) ) ;
#16304 = AXIS2_PLACEMENT_3D ( 'NONE', #18579, #4778, #10885 ) ;
#16305 = VERTEX_POINT ( 'NONE', #4630 ) ;
#16306 = CYLINDRICAL_SURFACE ( 'NONE', #1765, 1.000000000000000888 ) ;
#16307 = CIRCLE ( 'NONE', #13749, 5.700000000000001954 ) ;
#16308 = CYLINDRICAL_SURFACE ( 'NONE', #4497, 6.000000000000000888 ) ;
#16309 = ADVANCED_FACE ( 'NONE', ( #18338 ), #11838, .T. ) ;
#16310 = DIRECTION ( 'NONE',  ( 1.000000000000000000, 0.000000000000000000, 0.000000000000000000 ) ) ;
#16311 = FACE_OUTER_BOUND ( 'NONE', #17758, .T. ) ;
#16312 = EDGE_LOOP ( 'NONE', ( #16949, #9494, #16760, #10829 ) ) ;
#16313 = CARTESIAN_POINT ( 'NONE',  ( 6.968749997951614539, 0.7741991708318887166, -4.888101187500000222 ) ) ;
#16314 = CARTESIAN_POINT ( 'NONE',  ( -19.00000000000000355, 4.898587196589412829E-16, 0.000000000000000000 ) ) ;
#16315 = EDGE_CURVE ( 'NONE', #19129, #18274, #7979, .T. ) ;
#16316 = CARTESIAN_POINT ( 'NONE',  ( 8.500000000000007105, -4.080749450109678378, 4.080749450109621534 ) ) ;
#16317 = ORIENTED_EDGE ( 'NONE', *, *, #1887, .F. ) ;
#16318 = CARTESIAN_POINT ( 'NONE',  ( 2.783025342027733995, 5.408388659524090869, 23.92335783895639523 ) ) ;
#16319 = ORIENTED_EDGE ( 'NONE', *, *, #790, .F. ) ;
#16320 = AXIS2_PLACEMENT_3D ( 'NONE', #15597, #17290, #3487 ) ;
#16321 =( GEOMETRIC_REPRESENTATION_CONTEXT ( 3 ) GLOBAL_UNCERTAINTY_ASSIGNED_CONTEXT ( ( #2387 ) ) GLOBAL_UNIT_ASSIGNED_CONTEXT ( ( #7591, #17107, #15606 ) ) REPRESENTATION_CONTEXT ( 'NONE', 'WORKASPACE' ) );
#16322 = CARTESIAN_POINT ( 'NONE',  ( 3.954556930911861112, 2.873153789725825913, -14.84374999795161543 ) ) ;
#16323 = CARTESIAN_POINT ( 'NONE',  ( -4.080749450109650844, 4.080749450109650844, -9.812499995903225525 ) ) ;
#16324 = CARTESIAN_POINT ( 'NONE',  ( -16.28688694438836038, -7.664027248171298545, 35.00000000000000000 ) ) ;
#16325 = ORIENTED_EDGE ( 'NONE', *, *, #5657, .T. ) ;
#16326 = CARTESIAN_POINT ( 'NONE',  ( -4.620319390059841602, -1.773574444220693325, -11.96874999795161365 ) ) ;
#16327 = DIRECTION ( 'NONE',  ( -1.000000000000000000, 0.000000000000000000, 0.000000000000000000 ) ) ;
#16328 = ORIENTED_EDGE ( 'NONE', *, *, #13163, .T. ) ;
#16329 = B_SPLINE_CURVE_WITH_KNOTS ( 'NONE', 3,
 ( #13407, #9012, #10614, #1412 ),
 .UNSPECIFIED., .F., .F.,
 ( 4, 4 ),
 ( 0.005258139959819238193, 0.005342776758202895035 ),
 .UNSPECIFIED. ) ;
#16330 = VECTOR ( 'NONE', #14954, 1000.000000000000227 ) ;
#16331 = LINE ( 'NONE', #4125, #17950 ) ;
#16332 = CARTESIAN_POINT ( 'NONE',  ( 3.954556930911842016, -2.873153789725853002, -8.843749997951615427 ) ) ;
#16333 = ORIENTED_EDGE ( 'NONE', *, *, #19720, .F. ) ;
#16334 = CARTESIAN_POINT ( 'NONE',  ( 4.465502636338025688, -1.988169868018592856, -14.84374999795161543 ) ) ;
#16335 = CARTESIAN_POINT ( 'NONE',  ( 10.84374999795161543, 3.632567103900524064, 3.270778111535338262 ) ) ;
#16336 = DIRECTION ( 'NONE',  ( -1.000000000000000000, -0.000000000000000000, -0.000000000000000000 ) ) ;
#16337 = EDGE_CURVE ( 'NONE', #9696, #10889, #13736, .T. ) ;
#16338 = ORIENTED_EDGE ( 'NONE', *, *, #16122, .F. ) ;
#16339 = DIRECTION ( 'NONE',  ( -1.000000000000000000, -0.000000000000000000, -0.000000000000000000 ) ) ;
#16340 = ORIENTED_EDGE ( 'NONE', *, *, #13998, .F. ) ;
#16341 = CARTESIAN_POINT ( 'NONE',  ( -2.000000000000001776, -3.218695387886215453, -3.000000000000001776 ) ) ;
#16342 = ORIENTED_EDGE ( 'NONE', *, *, #9192, .T. ) ;
#16343 = CARTESIAN_POINT ( 'NONE',  ( 2.999999999999998224, -3.950217066951263956, -3.681818181818183877 ) ) ;
#16344 = LINE ( 'NONE', #2345, #19209 ) ;
#16345 = DIRECTION ( 'NONE',  ( 0.000000000000000000, 0.000000000000000000, -1.000000000000000000 ) ) ;
#16346 = DIRECTION ( 'NONE',  ( 0.5000000000000009992, 0.8660254037844380415, -0.000000000000000000 ) ) ;
#16347 = CIRCLE ( 'NONE', #7706, 4.200000000000000178 ) ;
#16348 = AXIS2_PLACEMENT_3D ( 'NONE', #7806, #12420, #7603 ) ;
#16349 = CARTESIAN_POINT ( 'NONE',  ( 1.000000000000003331, 18.00000000000000355, 35.00000000000000000 ) ) ;
#16350 = EDGE_CURVE ( 'NONE', #9124, #1853, #8841, .T. ) ;
#16351 = VERTEX_POINT ( 'NONE', #2919 ) ;
#16352 = VECTOR ( 'NONE', #19149, 1000.000000000000000 ) ;
#16353 = DIRECTION ( 'NONE',  ( 1.000000000000000000, 0.000000000000000000, 0.000000000000000000 ) ) ;
#16354 = ORIENTED_EDGE ( 'NONE', *, *, #10234, .T. ) ;
#16355 = EDGE_CURVE ( 'NONE', #9831, #18489, #16129, .T. ) ;
#16356 = CARTESIAN_POINT ( 'NONE',  ( 10.58013454126452046, -14.56230589874905412, 32.00000000000000000 ) ) ;
#16357 = AXIS2_PLACEMENT_3D ( 'NONE', #14320, #3709, #4915 ) ;
#16358 = CIRCLE ( 'NONE', #17963, 8.800000000000022027 ) ;
#16359 = CYLINDRICAL_SURFACE ( 'NONE', #12445, 28.06981291497571362 ) ;
#16360 = AXIS2_PLACEMENT_3D ( 'NONE', #11231, #9846, #14233 ) ;
#16361 = CARTESIAN_POINT ( 'NONE',  ( -3.000000000000002665, 0.000000000000000000, 0.000000000000000000 ) ) ;
#16362 = ORIENTED_EDGE ( 'NONE', *, *, #667, .T. ) ;
#16363 = FACE_OUTER_BOUND ( 'NONE', #8520, .T. ) ;
#16364 = MANIFOLD_SOLID_BREP ( 'Thread1', #16073 ) ;
#16365 = CARTESIAN_POINT ( 'NONE',  ( 2.597609400479564449E-15, -9.358633837799519082E-30, -41.79000000000000625 ) ) ;
#16366 = CARTESIAN_POINT ( 'NONE',  ( 3.143139765844623401, 4.840010801796480244, -9.500000000000003553 ) ) ;
#16367 = CIRCLE ( 'NONE', #14469, 24.12539914357697413 ) ;
#16368 = EDGE_LOOP ( 'NONE', ( #7652, #12367, #19348, #7484, #18654, #13747 ) ) ;
#16369 = ORIENTED_EDGE ( 'NONE', *, *, #9391, .T. ) ;
#16370 = CARTESIAN_POINT ( 'NONE',  ( 1.394999999999999574, 4.633866840648922292, 27.68468304288260384 ) ) ;
#16371 = CARTESIAN_POINT ( 'NONE',  ( 0.6764999999999817826, 0.000000000000000000, 0.000000000000000000 ) ) ;
#16372 = EDGE_CURVE ( 'NONE', #17740, #12265, #10550, .T. ) ;
#16373 = ORIENTED_EDGE ( 'NONE', *, *, #265, .F. ) ;
#16374 = CARTESIAN_POINT ( 'NONE',  ( -5.700000000000000178, -2.180340287075187351E-16, -13.97977757194593273 ) ) ;
#16375 = CIRCLE ( 'NONE', #8392, 30.00000000000000000 ) ;
#16376 = VERTEX_POINT ( 'NONE', #16449 ) ;
#16377 = CARTESIAN_POINT ( 'NONE',  ( -11.32184790671638730, 13.12143529358541549, 32.00000000000000000 ) ) ;
#16378 = VECTOR ( 'NONE', #1778, 1000.000000000000000 ) ;
#16379 = CARTESIAN_POINT ( 'NONE',  ( 0.000000000000000000, -5.535312321042547445, -23.48180575137738302 ) ) ;
#16380 = VERTEX_POINT ( 'NONE', #14941 ) ;
#16381 = DIRECTION ( 'NONE',  ( 0.000000000000000000, 0.000000000000000000, -1.000000000000000000 ) ) ;
#16382 = AXIS2_PLACEMENT_3D ( 'NONE', #6831, #17555, #13051 ) ;
#16383 = DIRECTION ( 'NONE',  ( 1.000000000000000000, 0.000000000000000000, 0.000000000000000000 ) ) ;
#16384 = CARTESIAN_POINT ( 'NONE',  ( 8.343749997951611874, 2.246813503491833508, -4.409619785863906571 ) ) ;
#16385 = EDGE_CURVE ( 'NONE', #3618, #4586, #2233, .T. ) ;
#16386 = EDGE_CURVE ( 'NONE', #18676, #16477, #11345, .T. ) ;
#16387 = CARTESIAN_POINT ( 'NONE',  ( 2.030753602223782206, -27.14986936243577986, 4.828194074574245320 ) ) ;
#16388 = CIRCLE ( 'NONE', #7758, 4.000000000000000000 ) ;
#16389 = CARTESIAN_POINT ( 'NONE',  ( 1.039999999999996927, 4.633866840649313090, -27.68468304288253634 ) ) ;
#16390 = FILL_AREA_STYLE_COLOUR ( '', #1667 ) ;
#16391 = ORIENTED_EDGE ( 'NONE', *, *, #13359, .F. ) ;
#16392 = DIRECTION ( 'NONE',  ( 1.000000000000000000, 0.000000000000000000, 0.000000000000000000 ) ) ;
#16393 = ADVANCED_FACE ( 'NONE', ( #17040 ), #1277, .T. ) ;
#16394 = LINE ( 'NONE', #16108, #437 ) ;
#16395 = CONICAL_SURFACE ( 'NONE', #10337, 4.762500000000000178, 0.9599310885968813656 ) ;
#16396 = UNCERTAINTY_MEASURE_WITH_UNIT (LENGTH_MEASURE( 1.000000000000000082E-05 ), #14717, 'distance_accuracy_value', 'NONE');
#16397 = DIRECTION ( 'NONE',  ( -1.000000000000000000, 0.000000000000000000, 0.000000000000000000 ) ) ;
#16398 = AXIS2_PLACEMENT_3D ( 'NONE', #14698, #19286, #5576 ) ;
#16399 =( BOUNDED_SURFACE ( )  B_SPLINE_SURFACE ( 1, 2, ( 
 ( #5197, #5302, #12714, #6586, #9920, #19102, #9823, #6687, #17311, #3606, #11410, #5486, #9727, #15815, #17510, #14519, #2393 ),
 ( #14614, #8206, #11316, #6882, #3896, #902, #2101, #14311, #17418, #5396, #19196, #8409, #15914, #10019, #2195, #8303, #16117 ) ),
 .UNSPECIFIED., .F., .F., .F. ) 
 B_SPLINE_SURFACE_WITH_KNOTS ( ( 2, 2 ),
 ( 3, 2, 2, 2, 2, 2, 2, 2, 3 ),
 ( 0.000000000000000000, 1.000000000000000000 ),
 ( 0.000000000000000000, 0.05000000000000000278, 0.1000000000000000056, 0.1499999999999999944, 0.2000000000000000111, 0.2500000000000000000, 0.2999999999999999889, 0.3499999999999999778, 0.4000000000000000222 ),
 .UNSPECIFIED. ) 
 GEOMETRIC_REPRESENTATION_ITEM ( )  RATIONAL_B_SPLINE_SURFACE ( (
 ( 1.000000000000000000, 0.9876883405951377704, 1.000000000000000000, 0.9876883405951377704, 1.000000000000000000, 0.9876883405951377704, 1.000000000000000000, 0.9876883405951377704, 1.000000000000000000, 0.9876883405951377704, 1.000000000000000000, 0.9876883405951377704, 1.000000000000000000, 0.9876883405951377704, 1.000000000000000000, 0.9876883405951377704, 1.000000000000000000),
 ( 1.000000000000000000, 0.9876883405951377704, 1.000000000000000000, 0.9876883405951377704, 1.000000000000000000, 0.9876883405951377704, 1.000000000000000000, 0.9876883405951377704, 1.000000000000000000, 0.9876883405951377704, 1.000000000000000000, 0.9876883405951377704, 1.000000000000000000, 0.9876883405951377704, 1.000000000000000000, 0.9876883405951377704, 1.000000000000000000) ) ) 
 REPRESENTATION_ITEM ( '' )  SURFACE ( )  );
#16400 = CARTESIAN_POINT ( 'NONE',  ( 4.780397808154265960, 1.280903732194420996, -8.968749997951613651 ) ) ;
#16401 = CARTESIAN_POINT ( 'NONE',  ( 6.656249997951614539, -4.936344801571268093, -2.850000000000058265 ) ) ;
#16402 = ORIENTED_EDGE ( 'NONE', *, *, #18860, .F. ) ;
#16403 = CARTESIAN_POINT ( 'NONE',  ( 0.5279272304333941790, -24.43806413951667622, -11.57956866523244166 ) ) ;
#16404 = DIRECTION ( 'NONE',  ( -0.000000000000000000, 0.000000000000000000, 1.000000000000000000 ) ) ;
#16405 =( GEOMETRIC_REPRESENTATION_CONTEXT ( 3 ) GLOBAL_UNCERTAINTY_ASSIGNED_CONTEXT ( ( #8791 ) ) GLOBAL_UNIT_ASSIGNED_CONTEXT ( ( #17620, #4010, #19405 ) ) REPRESENTATION_CONTEXT ( 'NONE', 'WORKASPACE' ) );
#16406 = ORIENTED_EDGE ( 'NONE', *, *, #9638, .F. ) ;
#16407 = CARTESIAN_POINT ( 'NONE',  ( 8.468749997951615427, -1.988169868018530462, -4.465502636338051445 ) ) ;
#16408 = CARTESIAN_POINT ( 'NONE',  ( 14.31249999590322552, 0.5958122406256767256, -5.668774803599153422 ) ) ;
#16409 = B_SPLINE_CURVE_WITH_KNOTS ( 'NONE', 3,
 ( #8696, #2298, #17705, #812 ),
 .UNSPECIFIED., .F., .F.,
 ( 4, 4 ),
 ( 2.034713381942717623E-07, 0.0006887909409525219510 ),
 .UNSPECIFIED. ) ;
#16410 = AXIS2_PLACEMENT_3D ( 'NONE', #9503, #14192, #15504 ) ;
#16411 = CARTESIAN_POINT ( 'NONE',  ( 13.32184790671640151, 13.12143529358541016, -32.00000000000000000 ) ) ;
#16412 = FACE_OUTER_BOUND ( 'NONE', #12363, .T. ) ;
#16413 = VERTEX_POINT ( 'NONE', #5022 ) ;
#16414 = CARTESIAN_POINT ( 'NONE',  ( -19.00000000000000355, -3.434748899119118182, 2.750000000000001776 ) ) ;
#16415 = CARTESIAN_POINT ( 'NONE',  ( 4.233219804643871598, -2.444050593750019651, -11.84374999795161365 ) ) ;
#16416 = FACE_OUTER_BOUND ( 'NONE', #4798, .T. ) ;
#16417 = ORIENTED_EDGE ( 'NONE', *, *, #11909, .F. ) ;
#16418 = CARTESIAN_POINT ( 'NONE',  ( 0.7589665326895891351, 12.98167595241022276, 24.32849926382755257 ) ) ;
#16419 =( GEOMETRIC_REPRESENTATION_CONTEXT ( 3 ) GLOBAL_UNCERTAINTY_ASSIGNED_CONTEXT ( ( #6780 ) ) GLOBAL_UNIT_ASSIGNED_CONTEXT ( ( #9507, #18794, #1794 ) ) REPRESENTATION_CONTEXT ( 'NONE', 'WORKASPACE' ) );
#16420 = ORIENTED_EDGE ( 'NONE', *, *, #4774, .T. ) ;
#16421 = CARTESIAN_POINT ( 'NONE',  ( -11.00000000000000355, -4.898587196589412829E-16, 0.000000000000000000 ) ) ;
#16422 = ADVANCED_FACE ( 'NONE', ( #17135 ), #322, .T. ) ;
#16423 = CARTESIAN_POINT ( 'NONE',  ( 6.468749997951615427, 0.000000000000000000, -4.888101187500000222 ) ) ;
#16424 = ADVANCED_FACE ( 'NONE', ( #14231 ), #9639, .F. ) ;
#16425 = PRODUCT_DEFINITION_SHAPE ( 'NONE', 'NONE',  #12983 ) ;
#16426 = CARTESIAN_POINT ( 'NONE',  ( -90.00000000000000000, 0.000000000000000000, -6.000000000000021316 ) ) ;
#16427 = DIRECTION ( 'NONE',  ( 0.000000000000000000, 0.000000000000000000, -1.000000000000000000 ) ) ;
#16428 = EDGE_LOOP ( 'NONE', ( #19593, #4357 ) ) ;
#16429 = VECTOR ( 'NONE', #13374, 1000.000000000000000 ) ;
#16430 = CARTESIAN_POINT ( 'NONE',  ( 2.765633920072239516, 16.37294372382858398, 18.55949924794898465 ) ) ;
#16431 = FACE_OUTER_BOUND ( 'NONE', #8253, .T. ) ;
#16432 = ORIENTED_EDGE ( 'NONE', *, *, #4521, .F. ) ;
#16433 = EDGE_CURVE ( 'NONE', #7960, #16090, #15622, .T. ) ;
#16434 = AXIS2_PLACEMENT_3D ( 'NONE', #6945, #19162, #2359 ) ;
#16435 = CARTESIAN_POINT ( 'NONE',  ( 12.32184790671639618, 13.12143529358541016, 35.00000000000000000 ) ) ;
#16436 = CARTESIAN_POINT ( 'NONE',  ( 2.620002426024508502, -5.142044285764769462, -10.81249999590322375 ) ) ;
#16437 = ADVANCED_FACE ( 'NONE', ( #11133, #1922 ), #12732, .T. ) ;
#16438 = ORIENTED_EDGE ( 'NONE', *, *, #4503, .T. ) ;
#16439 = CARTESIAN_POINT ( 'NONE',  ( -90.00000000000000000, 0.000000000000000000, 0.000000000000000000 ) ) ;
#16440 = CARTESIAN_POINT ( 'NONE',  ( 13.00000000000000178, 0.7793280607715257213, 4.825575716215943167 ) ) ;
#16441 = ADVANCED_FACE ( 'NONE', ( #7720 ), #325, .F. ) ;
#16442 = CARTESIAN_POINT ( 'NONE',  ( 90.56249999999998579, 0.000000000000000000, 0.000000000000000000 ) ) ;
#16443 = AXIS2_PLACEMENT_3D ( 'NONE', #12923, #2594, #2497 ) ;
#16444 = ORIENTED_EDGE ( 'NONE', *, *, #7346, .F. ) ;
#16445 = CARTESIAN_POINT ( 'NONE',  ( 0.1882239080259267838, -25.40949241676349146, -5.251266773802644394 ) ) ;
#16446 = ORIENTED_EDGE ( 'NONE', *, *, #12271, .T. ) ;
#16447 = DIRECTION ( 'NONE',  ( 1.000000000000000000, 0.000000000000000000, 0.000000000000000000 ) ) ;
#16448 = EDGE_LOOP ( 'NONE', ( #15467, #18629 ) ) ;
#16449 = CARTESIAN_POINT ( 'NONE',  ( 2.789999999999999147, 12.52067188844381107, -20.62201879784899461 ) ) ;
#16450 = CARTESIAN_POINT ( 'NONE',  ( -19.00000000000000355, 4.898587196589412829E-16, 0.000000000000000000 ) ) ;
#16451 = DIRECTION ( 'NONE',  ( -0.000000000000000000, -0.000000000000000000, 1.000000000000000000 ) ) ;
#16452 = CARTESIAN_POINT ( 'NONE',  ( 12.50000000000000533, -0.3020334839682081163, -5.763142191869158992 ) ) ;
#16453 = AXIS2_PLACEMENT_3D ( 'NONE', #16171, #14757, #19539 ) ;
#16454 = DIRECTION ( 'NONE',  ( 0.000000000000000000, 0.000000000000000000, 1.000000000000000000 ) ) ;
#16455 = ORIENTED_EDGE ( 'NONE', *, *, #19594, .T. ) ;
#16456 = CARTESIAN_POINT ( 'NONE',  ( 13.00000000000000000, -4.125339889944092953, 2.622041954598548941 ) ) ;
#16457 = CARTESIAN_POINT ( 'NONE',  ( 2.257825467309740208, -3.467596033028475855, 26.83036154824992892 ) ) ;
#16458 = VECTOR ( 'NONE', #6572, 1000.000000000000000 ) ;
#16459 = EDGE_CURVE ( 'NONE', #3194, #768, #645, .T. ) ;
#16460 = ORIENTED_EDGE ( 'NONE', *, *, #13746, .F. ) ;
#16461 = DIRECTION ( 'NONE',  ( -1.000000000000000000, -0.000000000000000000, -0.000000000000000000 ) ) ;
#16462 = EDGE_CURVE ( 'NONE', #18644, #3152, #963, .T. ) ;
#16463 = AXIS2_PLACEMENT_3D ( 'NONE', #3873, #6663, #788 ) ;
#16464 = FACE_OUTER_BOUND ( 'NONE', #19680, .T. ) ;
#16465 = FACE_OUTER_BOUND ( 'NONE', #8506, .T. ) ;
#16466 = DIRECTION ( 'NONE',  ( 0.000000000000000000, 0.000000000000000000, 1.000000000000000000 ) ) ;
#16467 = EDGE_LOOP ( 'NONE', ( #11224, #8637 ) ) ;
#16468 = CARTESIAN_POINT ( 'NONE',  ( 2.783068945535914995, 2.248820353272968919, 24.42321038836783131 ) ) ;
#16469 = DIRECTION ( 'NONE',  ( 0.000000000000000000, 0.000000000000000000, 1.000000000000000000 ) ) ;
#16470 = CARTESIAN_POINT ( 'NONE',  ( -4.942249507334558700, -0.2590123213420631454, -12.96874999795161543 ) ) ;
#16471 = CARTESIAN_POINT ( 'NONE',  ( -0.5958122406256771697, -5.668774803599153422, -9.312499995903225525 ) ) ;
#16472 = ORIENTED_EDGE ( 'NONE', *, *, #17807, .T. ) ;
#16473 = EDGE_LOOP ( 'NONE', ( #5093, #14123, #10933, #16225, #17635 ) ) ;
#16474 = DIRECTION ( 'NONE',  ( 0.000000000000000000, 0.000000000000000000, 1.000000000000000000 ) ) ;
#16475 = EDGE_CURVE ( 'NONE', #1013, #5836, #7012, .T. ) ;
#16476 = CARTESIAN_POINT ( 'NONE',  ( 0.000000000000000000, 4.999999999999998224, 41.99999999999999289 ) ) ;
#16477 = VERTEX_POINT ( 'NONE', #8015 ) ;
#16478 = CIRCLE ( 'NONE', #10409, 4.200000000000000178 ) ;
#16479 = CARTESIAN_POINT ( 'NONE',  ( -10.58013454126452224, -14.56230589874905235, -32.00000000000000000 ) ) ;
#16480 = EDGE_LOOP ( 'NONE', ( #11174, #1167 ) ) ;
#16481 = AXIS2_PLACEMENT_3D ( 'NONE', #4367, #8666, #7550 ) ;
#16482 = FACE_OUTER_BOUND ( 'NONE', #10563, .T. ) ;
#16483 = EDGE_CURVE ( 'NONE', #18724, #5844, #14129, .T. ) ;
#16484 = DIRECTION ( 'NONE',  ( -1.000000000000000000, -0.000000000000000000, -0.000000000000000000 ) ) ;
#16485 = ORIENTED_EDGE ( 'NONE', *, *, #10679, .T. ) ;
#16486 = CARTESIAN_POINT ( 'NONE',  ( 0.000000000000000000, 1.991882183130641248, -24.04302995059964942 ) ) ;
#16487 = EDGE_CURVE ( 'NONE', #5305, #4629, #19477, .T. ) ;
#16488 = FACE_BOUND ( 'NONE', #2819, .T. ) ;
#16489 = CARTESIAN_POINT ( 'NONE',  ( 10.34374999795161543, 4.409619785863906571, -2.246813503491833508 ) ) ;
#16490 = CARTESIAN_POINT ( 'NONE',  ( -1.799999999999999600, 0.000000000000000000, 0.000000000000000000 ) ) ;
#16491 = LINE ( 'NONE', #10490, #6285 ) ;
#16492 = SURFACE_STYLE_USAGE ( .BOTH. , #12285 ) ;
#16493 = CARTESIAN_POINT ( 'NONE',  ( 6.000000000000005329, 0.000000000000000000, 0.000000000000000000 ) ) ;
#16494 = AXIS2_PLACEMENT_3D ( 'NONE', #18324, #15618, #9824 ) ;
#16495 = ORIENTED_EDGE ( 'NONE', *, *, #979, .F. ) ;
#16496 = DIRECTION ( 'NONE',  ( 1.000000000000000000, 0.000000000000000000, 0.000000000000000000 ) ) ;
#16497 = FACE_OUTER_BOUND ( 'NONE', #7050, .T. ) ;
#16498 = CARTESIAN_POINT ( 'NONE',  ( -2.444050593749990341, 4.233219804643887585, -6.468749997951615427 ) ) ;
#16499 = CARTESIAN_POINT ( 'NONE',  ( -3.631840208645857437, -4.484949146646330931, -7.812499995903224637 ) ) ;
#16500 = ORIENTED_EDGE ( 'NONE', *, *, #13187, .F. ) ;
#16501 = FACE_OUTER_BOUND ( 'NONE', #10209, .T. ) ;
#16502 = EDGE_CURVE ( 'NONE', #10379, #12338, #14693, .T. ) ;
#16503 = CARTESIAN_POINT ( 'NONE',  ( -2.444050593750049849, -4.233219804643852946, -6.468749997951615427 ) ) ;
#16504 = AXIS2_PLACEMENT_3D ( 'NONE', #1619, #17030, #15335 ) ;
#16505 = ORIENTED_EDGE ( 'NONE', *, *, #6861, .F. ) ;
#16506 = CARTESIAN_POINT ( 'NONE',  ( 7.812499995903224637, 4.484949146646356688, 3.631840208645826795 ) ) ;
#16507 = CIRCLE ( 'NONE', #17149, 28.06981291497571007 ) ;
#16508 = CARTESIAN_POINT ( 'NONE',  ( 6.843749997951615427, -4.233219804643904460, 2.444050593749960587 ) ) ;
#16509 = ADVANCED_FACE ( 'NONE', ( #17233 ), #10866, .T. ) ;
#16510 = CARTESIAN_POINT ( 'NONE',  ( -7.937500000000000000, 4.582717761692651770, -0.7089489049740185234 ) ) ;
#16511 = CARTESIAN_POINT ( 'NONE',  ( 2.789999999999999147, 21.30679549418631780, 12.59161484032919986 ) ) ;
#16512 = ORIENTED_EDGE ( 'NONE', *, *, #8732, .F. ) ;
#16513 = CARTESIAN_POINT ( 'NONE',  ( 9.468749997951615427, 3.954556930911862000, -2.873153789725825469 ) ) ;
#16514 = LINE ( 'NONE', #16715, #4296 ) ;
#16515 = CARTESIAN_POINT ( 'NONE',  ( 12.86923836996420967, -11.47363181547641453, 35.00000000000000000 ) ) ;
#16516 = VERTEX_POINT ( 'NONE', #18532 ) ;
#16517 =( BOUNDED_CURVE ( )  B_SPLINE_CURVE ( 2, ( #19086, #10096, #19279, #4083, #10188, #5473, #16289, #794, #14886, #5377, #19180, #11585, #14600, #17884, #17788 ),
 .UNSPECIFIED., .F., .F. ) 
 B_SPLINE_CURVE_WITH_KNOTS ( ( 3, 2, 2, 2, 2, 2, 2, 3 ),
 ( 0.000000000000000000, 0.05000000000000000278, 0.1000000000000000056, 0.1499999999999999944, 0.2000000000000000111, 0.2500000000000000000, 0.2999999999999999889, 0.3078686208676164604 ),
 .UNSPECIFIED. ) 
 CURVE ( )  GEOMETRIC_REPRESENTATION_ITEM ( )  RATIONAL_B_SPLINE_CURVE ( ( 1.000000000000000000, 0.9876883405951377704, 1.000000000000000000, 0.9876883405951377704, 1.000000000000000000, 0.9876883405951377704, 1.000000000000000000, 0.9876883405951377704, 1.000000000000000000, 0.9876883405951377704, 1.000000000000000000, 0.9876883405951377704, 1.000000000000000000, 0.9980624843978382899, 0.9967347918236166837 ) ) 
 REPRESENTATION_ITEM ( '' )  );
#16518 = CARTESIAN_POINT ( 'NONE',  ( 5.000000000000000000, -2.000000000000001776, 37.99999999999999289 ) ) ;
#16519 = CIRCLE ( 'NONE', #2131, 1.000000000000000888 ) ;
#16520 = ORIENTED_EDGE ( 'NONE', *, *, #3108, .T. ) ;
#16521 = CARTESIAN_POINT ( 'NONE',  ( -0.000000000000000000, 0.000000000000000000, 0.000000000000000000 ) ) ;
#16522 = AXIS2_PLACEMENT_3D ( 'NONE', #3916, #16140, #17628 ) ;
#16523 = B_SPLINE_CURVE_WITH_KNOTS ( 'NONE', 3,
 ( #10981, #367, #1872, #6069 ),
 .UNSPECIFIED., .F., .F.,
 ( 4, 4 ),
 ( 0.005258139959819248602, 0.005948405594583415848 ),
 .UNSPECIFIED. ) ;
#16524 = CARTESIAN_POINT ( 'NONE',  ( 13.00000000000000178, 0.000000000000000000, 0.000000000000000000 ) ) ;
#16525 = CARTESIAN_POINT ( 'NONE',  ( 13.00000000000000533, -4.560365019702126155, -2.978280878416461164 ) ) ;
#16526 = CARTESIAN_POINT ( 'NONE',  ( 13.32184790671640151, 13.12143529358541016, -32.00000000000000000 ) ) ;
#16527 = ORIENTED_EDGE ( 'NONE', *, *, #12390, .T. ) ;
#16528 = CARTESIAN_POINT ( 'NONE',  ( -4.781284448697201483, -1.016293382781378485, -12.46874999795161543 ) ) ;
#16529 = EDGE_CURVE ( 'NONE', #9896, #5740, #7321, .T. ) ;
#16530 = LINE ( 'NONE', #3111, #3072 ) ;
#16531 = ORIENTED_EDGE ( 'NONE', *, *, #13377, .T. ) ;
#16532 = TOROIDAL_SURFACE ( 'NONE', #14610, 24.12539914357697413, 8.000000000000000000 ) ;
#16533 = AXIS2_PLACEMENT_3D ( 'NONE', #11768, #16275, #8199 ) ;
#16534 = EDGE_CURVE ( 'NONE', #11113, #15383, #6529, .T. ) ;
#16535 = CARTESIAN_POINT ( 'NONE',  ( 3.499494075959815653, 3.499494075959816541, -14.34374999795161365 ) ) ;
#16536 = EDGE_CURVE ( 'NONE', #18719, #19366, #5577, .T. ) ;
#16537 = ORIENTED_EDGE ( 'NONE', *, *, #17312, .T. ) ;
#16538 = CARTESIAN_POINT ( 'NONE',  ( 91.50000000000000000, 0.000000000000000000, 3.593999999999999861 ) ) ;
#16539 = CARTESIAN_POINT ( 'NONE',  ( 7.671566133830872047, 15.77352024078954784, -35.00000000000000000 ) ) ;
#16540 = CARTESIAN_POINT ( 'NONE',  ( 12.46874999795161543, 4.648860486681953397, 1.510506337161861223 ) ) ;
#16541 = ORIENTED_EDGE ( 'NONE', *, *, #14616, .F. ) ;
#16542 = DIRECTION ( 'NONE',  ( 0.000000000000000000, 0.000000000000000000, 1.000000000000000000 ) ) ;
#16543 = ORIENTED_EDGE ( 'NONE', *, *, #16757, .F. ) ;
#16544 = CARTESIAN_POINT ( 'NONE',  ( 0.07186813532171117125, -25.22589920183359169, -2.577209017047271011 ) ) ;
#16545 = ORIENTED_EDGE ( 'NONE', *, *, #17194, .T. ) ;
#16546 = SURFACE_STYLE_FILL_AREA ( #17946 ) ;
#16547 = CARTESIAN_POINT ( 'NONE',  ( 0.000000000000000000, 0.000000000000000000, -35.00000000000000000 ) ) ;
#16548 = EDGE_CURVE ( 'NONE', #2502, #1264, #10225, .T. ) ;
#16549 = LINE ( 'NONE', #19439, #6017 ) ;
#16550 = FACE_OUTER_BOUND ( 'NONE', #6445, .T. ) ;
#16551 = AXIS2_PLACEMENT_3D ( 'NONE', #8613, #17433, #8224 ) ;
#16552 = CARTESIAN_POINT ( 'NONE',  ( 2.850000000000024070, 4.936344801571289409, -7.312499995903225525 ) ) ;
#16553 = AXIS2_PLACEMENT_3D ( 'NONE', #1312, #7389, #4410 ) ;
#16554 = ORIENTED_EDGE ( 'NONE', *, *, #6938, .T. ) ;
#16555 = CARTESIAN_POINT ( 'NONE',  ( 2.604434404052931473, -17.45907811351440841, -19.17825124759797006 ) ) ;
#16556 = ADVANCED_FACE ( 'NONE', ( #14433 ), #8431, .F. ) ;
#16557 = DIRECTION ( 'NONE',  ( -1.000000000000000000, -0.000000000000000000, -0.000000000000000000 ) ) ;
#16558 = ORIENTED_EDGE ( 'NONE', *, *, #9301, .T. ) ;
#16559 = CARTESIAN_POINT ( 'NONE',  ( 0.02436607992776411782, -16.37294372382844543, -18.55949924794910544 ) ) ;
#16560 = CARTESIAN_POINT ( 'NONE',  ( -11.00000000000000355, -4.200000000000001066, 0.000000000000000000 ) ) ;
#16561 = VECTOR ( 'NONE', #9090, 1000.000000000000000 ) ;
#16562 = ORIENTED_EDGE ( 'NONE', *, *, #5520, .T. ) ;
#16563 = DIRECTION ( 'NONE',  ( -1.000000000000000000, -0.000000000000000000, -0.000000000000000000 ) ) ;
#16564 = CYLINDRICAL_SURFACE ( 'NONE', #19031, 6.735000000000022524 ) ;
#16565 = AXIS2_PLACEMENT_3D ( 'NONE', #15493, #483, #15589 ) ;
#16566 = DIRECTION ( 'NONE',  ( 1.000000000000000000, 0.000000000000000000, 0.000000000000000000 ) ) ;
#16567 = EDGE_LOOP ( 'NONE', ( #11591, #10876 ) ) ;
#16568 = CARTESIAN_POINT ( 'NONE',  ( 10.46874999795161720, -3.632567103900500971, -3.270778111535363131 ) ) ;
#16569 = VERTEX_POINT ( 'NONE', #4015 ) ;
#16570 = CARTESIAN_POINT ( 'NONE',  ( 0.5958122406256382009, 5.668774803599156975, -8.000000000000005329 ) ) ;
#16571 = LINE ( 'NONE', #15064, #3508 ) ;
#16572 = VERTEX_POINT ( 'NONE', #14331 ) ;
#16573 = ORIENTED_EDGE ( 'NONE', *, *, #17824, .F. ) ;
#16574 = DIRECTION ( 'NONE',  ( 0.000000000000000000, 0.000000000000000000, 1.000000000000000000 ) ) ;
#16575 = CARTESIAN_POINT ( 'NONE',  ( -1.773574444220725521, 4.620319390059830056, -7.343749997951615427 ) ) ;
#16576 = EDGE_LOOP ( 'NONE', ( #11579, #321, #6501, #11958 ) ) ;
#16577 = CIRCLE ( 'NONE', #10820, 1.000000000000004441 ) ;
#16578 = CARTESIAN_POINT ( 'NONE',  ( 2.318398865532074193, 5.207209108562820710, -9.000000000000005329 ) ) ;
#16579 = EDGE_LOOP ( 'NONE', ( #292, #3530, #206, #6209 ) ) ;
#16580 = DIRECTION ( 'NONE',  ( 4.060088635510494296E-15, -1.000000000000000000, 0.000000000000000000 ) ) ;
#16581 = CARTESIAN_POINT ( 'NONE',  ( 0.1855657168891864939, -12.84444904262008436, -22.53097606932998787 ) ) ;
#16582 = EDGE_LOOP ( 'NONE', ( #9665, #16325, #4853, #7499, #13675, #13752, #2942, #17811, #6528, #15359 ) ) ;
#16583 = MECHANICAL_DESIGN_GEOMETRIC_PRESENTATION_REPRESENTATION (  '', ( #8593 ), #13705 ) ;
#16584 = DIRECTION ( 'NONE',  ( 1.000000000000000000, 0.000000000000000000, 0.000000000000000000 ) ) ;
#16585 = CARTESIAN_POINT ( 'NONE',  ( 12.31249999590322552, 5.700000000000001066, -3.490243377569957047E-16 ) ) ;
#16586 = DIRECTION ( 'NONE',  ( 0.000000000000000000, 0.000000000000000000, 1.000000000000000000 ) ) ;
#16587 = AXIS2_PLACEMENT_3D ( 'NONE', #15864, #8043, #5441 ) ;
#16588 = VERTEX_POINT ( 'NONE', #17821 ) ;
#16589 = CARTESIAN_POINT ( 'NONE',  ( -7.937500000000000000, 4.582717761692651770, -6.527800000000000047 ) ) ;
#16590 = SURFACE_STYLE_USAGE ( .BOTH. , #10491 ) ;
#16591 = VERTEX_POINT ( 'NONE', #16137 ) ;
#16592 = CARTESIAN_POINT ( 'NONE',  ( 16.28688694438835327, -7.664027248171309203, 32.00000000000000000 ) ) ;
#16593 = FACE_BOUND ( 'NONE', #15035, .T. ) ;
#16594 = UNCERTAINTY_MEASURE_WITH_UNIT (LENGTH_MEASURE( 1.000000000000000082E-05 ), #10079, 'distance_accuracy_value', 'NONE');
#16595 = DIRECTION ( 'NONE',  ( 0.000000000000000000, 0.000000000000000000, -1.000000000000000000 ) ) ;
#16596 = CARTESIAN_POINT ( 'NONE',  ( 3.114526743279282694, 3.846120219227923798, -6.968749997951614539 ) ) ;
#16597 = CARTESIAN_POINT ( 'NONE',  ( 12.99999999999999467, 4.444590484536241171, 2.035510078342908091 ) ) ;
#16598 = EDGE_CURVE ( 'NONE', #7172, #13172, #12151, .T. ) ;
#16599 = VERTEX_POINT ( 'NONE', #11617 ) ;
#16600 = LINE ( 'NONE', #13593, #10606 ) ;
#16601 = CARTESIAN_POINT ( 'NONE',  ( -4.781284448697179279, 1.016293382781477961, -10.46874999795161720 ) ) ;
#16602 = AXIS2_PLACEMENT_3D ( 'NONE', #5644, #15970, #8756 ) ;
#16603 = ORIENTED_EDGE ( 'NONE', *, *, #13662, .T. ) ;
#16604 = CARTESIAN_POINT ( 'NONE',  ( 9.812499995903223748, 1.493657965219485018, 5.574407415329170057 ) ) ;
#16605 = CARTESIAN_POINT ( 'NONE',  ( -5.668774803599153422, 0.5958122406256767256, -14.31249999590322552 ) ) ;
#16606 = CARTESIAN_POINT ( 'NONE',  ( 9.468749997951615427, -0.5109457054261099529, -4.861323657744413218 ) ) ;
#16607 = DIRECTION ( 'NONE',  ( 0.000000000000000000, 0.000000000000000000, 1.000000000000000000 ) ) ;
#16608 = ORIENTED_EDGE ( 'NONE', *, *, #3331, .F. ) ;
#16609 = FACE_OUTER_BOUND ( 'NONE', #18828, .T. ) ;
#16610 = DIRECTION ( 'NONE',  ( 0.000000000000000000, 0.000000000000000000, -1.000000000000000000 ) ) ;
#16611 = CARTESIAN_POINT ( 'NONE',  ( 8.000000000000005329, -3.350375938067129855, 4.611396867937178179 ) ) ;
#16612 = ORIENTED_EDGE ( 'NONE', *, *, #2002, .T. ) ;
#16613 = DIRECTION ( 'NONE',  ( 0.000000000000000000, 0.000000000000000000, 1.000000000000000000 ) ) ;
#16614 = CARTESIAN_POINT ( 'NONE',  ( 8.468749997951615427, -2.873153789725853002, 3.954556930911842016 ) ) ;
#16615 = CARTESIAN_POINT ( 'NONE',  ( 7.968749997951616315, 2.246813503491833508, -4.409619785863906571 ) ) ;
#16616 = CARTESIAN_POINT ( 'NONE',  ( 16.28688694438835327, -7.664027248171309203, -32.00000000000000000 ) ) ;
#16617 = AXIS2_PLACEMENT_3D ( 'NONE', #19215, #5508, #10037 ) ;
#16618 = DIRECTION ( 'NONE',  ( -0.000000000000000000, -0.000000000000000000, 1.000000000000000000 ) ) ;
#16619 = VECTOR ( 'NONE', #16024, 1000.000000000000000 ) ;
#16620 = EDGE_CURVE ( 'NONE', #17188, #10783, #2495, .T. ) ;
#16621 = ORIENTED_EDGE ( 'NONE', *, *, #2467, .T. ) ;
#16622 = PLANE ( 'NONE',  #7707 ) ;
#16623 = CYLINDRICAL_SURFACE ( 'NONE', #11065, 28.06981291497571362 ) ;
#16624 = ORIENTED_EDGE ( 'NONE', *, *, #16433, .T. ) ;
#16625 = CARTESIAN_POINT ( 'NONE',  ( -2.993098736590125853E-16, 4.888101187500000222, -11.46874999795161543 ) ) ;
#16626 = DIRECTION ( 'NONE',  ( 5.011428603230760289E-33, -0.7806247497997995666, 0.6250000000000002220 ) ) ;
#16627 =( BOUNDED_SURFACE ( )  B_SPLINE_SURFACE ( 1, 2, ( 
 ( #13614, #19414, #4500, #7597, #5796, #1309, #16722, #11917, #10617, #10329, #13511, #3103, #1211, #19782, #7288, #3002, #9116 ),
 ( #16423, #11815, #7494, #16615, #13408, #17922, #4311, #2700, #14919, #15219, #18029, #19712, #1513, #13713, #10422, #5996, #7387 ) ),
 .UNSPECIFIED., .F., .F., .F. ) 
 B_SPLINE_SURFACE_WITH_KNOTS ( ( 2, 2 ),
 ( 3, 2, 2, 2, 2, 2, 2, 2, 3 ),
 ( 0.000000000000000000, 1.000000000000000000 ),
 ( 0.000000000000000000, 0.05000000000000000278, 0.1000000000000000056, 0.1499999999999999944, 0.2000000000000000111, 0.2500000000000000000, 0.2999999999999999889, 0.3499999999999999778, 0.4000000000000000222 ),
 .UNSPECIFIED. ) 
 GEOMETRIC_REPRESENTATION_ITEM ( )  RATIONAL_B_SPLINE_SURFACE ( (
 ( 1.000000000000000000, 0.9876883405951377704, 1.000000000000000000, 0.9876883405951377704, 1.000000000000000000, 0.9876883405951377704, 1.000000000000000000, 0.9876883405951377704, 1.000000000000000000, 0.9876883405951377704, 1.000000000000000000, 0.9876883405951377704, 1.000000000000000000, 0.9876883405951377704, 1.000000000000000000, 0.9876883405951377704, 1.000000000000000000),
 ( 1.000000000000000000, 0.9876883405951377704, 1.000000000000000000, 0.9876883405951377704, 1.000000000000000000, 0.9876883405951377704, 1.000000000000000000, 0.9876883405951377704, 1.000000000000000000, 0.9876883405951377704, 1.000000000000000000, 0.9876883405951377704, 1.000000000000000000, 0.9876883405951377704, 1.000000000000000000, 0.9876883405951377704, 1.000000000000000000) ) ) 
 REPRESENTATION_ITEM ( '' )  SURFACE ( )  );
#16628 = ORIENTED_EDGE ( 'NONE', *, *, #15668, .T. ) ;
#16630 = CARTESIAN_POINT ( 'NONE',  ( 12.99999999999998757, 4.496303326521696064, -2.563255015864441155 ) ) ;
#16629 = AXIS2_PLACEMENT_3D ( 'NONE', #15413, #4904, #17600 ) ;
#16631 = CARTESIAN_POINT ( 'NONE',  ( 7.312499995903225525, 4.936344801571308061, -2.849999999999989431 ) ) ;
#16632 = COLOUR_RGB ( '', 0.40784314, 0.44705882, 0.49803922) ;
#16633 = FACE_OUTER_BOUND ( 'NONE', #11038, .T. ) ;
#16634 = ORIENTED_EDGE ( 'NONE', *, *, #18771, .F. ) ;
#16635 = ADVANCED_FACE ( 'NONE', ( #12932, #7091 ), #19027, .T. ) ;
#16636 = LINE ( 'NONE', #18046, #14711 ) ;
#16637 = ORIENTED_EDGE ( 'NONE', *, *, #16064, .F. ) ;
#16638 = ADVANCED_FACE ( 'NONE', ( #920 ), #13224, .T. ) ;
#16639 = CARTESIAN_POINT ( 'NONE',  ( -3.968750000000007994, -6.874076642538976323, 0.000000000000000000 ) ) ;
#16640 = EDGE_LOOP ( 'NONE', ( #17585, #15801 ) ) ;
#16641 = DIRECTION ( 'NONE',  ( 1.000000000000000000, 0.000000000000000000, 0.000000000000000000 ) ) ;
#16642 = CARTESIAN_POINT ( 'NONE',  ( -19.00000000000000355, -3.278623949159158890, 2.625000000000000888 ) ) ;
#16643 = DIRECTION ( 'NONE',  ( -1.000000000000000000, -0.000000000000000000, -0.000000000000000000 ) ) ;
#16644 = EDGE_CURVE ( 'NONE', #14651, #608, #16799, .T. ) ;
#16645 = CARTESIAN_POINT ( 'NONE',  ( 7.968749997951616315, 4.942249507334556924, -0.2590123213420971182 ) ) ;
#16646 = EDGE_LOOP ( 'NONE', ( #3502, #16651, #18444, #2583 ) ) ;
#16647 = DIRECTION ( 'NONE',  ( -1.000000000000000000, 0.000000000000000000, 0.000000000000000000 ) ) ;
#16648 = ADVANCED_FACE ( 'NONE', ( #14725, #629 ), #6706, .F. ) ;
#16649 = VECTOR ( 'NONE', #6462, 1000.000000000000000 ) ;
#16650 = FILL_AREA_STYLE ('',( #4536 ) ) ;
#16651 = ORIENTED_EDGE ( 'NONE', *, *, #16013, .F. ) ;
#16652 = CARTESIAN_POINT ( 'NONE',  ( -2.000000000000001776, 0.000000000000000000, 0.000000000000000000 ) ) ;
#16653 = EDGE_CURVE ( 'NONE', #9186, #16599, #9844, .T. ) ;
#16654 = DIRECTION ( 'NONE',  ( 1.000000000000000000, -0.000000000000000000, -0.000000000000000000 ) ) ;
#16655 = ORIENTED_EDGE ( 'NONE', *, *, #2311, .F. ) ;
#16656 = CARTESIAN_POINT ( 'NONE',  ( 1.039999999999997371, -4.147968289691092991, -27.76164181293055933 ) ) ;
#16657 = CARTESIAN_POINT ( 'NONE',  ( 4.861323657744411442, 0.5109457054261445919, -9.468749997951615427 ) ) ;
#16658 = CARTESIAN_POINT ( 'NONE',  ( 1.749999999999998002, -24.89775460606821866, -12.96210679857815684 ) ) ;
#16659 = ORIENTED_EDGE ( 'NONE', *, *, #3425, .T. ) ;
#16660 = CARTESIAN_POINT ( 'NONE',  ( 11.46874999795161543, -2.444050593749961031, -4.233219804643904460 ) ) ;
#16661 = CIRCLE ( 'NONE', #11552, 6.000000000000000000 ) ;
#16662 = EDGE_LOOP ( 'NONE', ( #16809, #9418, #7615, #18784 ) ) ;
#16663 = DIRECTION ( 'NONE',  ( 0.000000000000000000, 0.000000000000000000, 1.000000000000000000 ) ) ;
#16664 = AXIS2_PLACEMENT_3D ( 'NONE', #10044, #16144, #14543 ) ;
#16665 = EDGE_CURVE ( 'NONE', #3097, #8767, #3521, .T. ) ;
#16666 = DIRECTION ( 'NONE',  ( -1.000000000000000000, -0.000000000000000000, 0.000000000000000000 ) ) ;
#16667 = CARTESIAN_POINT ( 'NONE',  ( -3.143139765844656264, -4.840010801796461593, -10.81249999590322375 ) ) ;
#16668 = AXIS2_PLACEMENT_3D ( 'NONE', #16450, #1534, #4631 ) ;
#16669 = ORIENTED_EDGE ( 'NONE', *, *, #15902, .F. ) ;
#16670 = ORIENTED_EDGE ( 'NONE', *, *, #1981, .T. ) ;
#16671 = LINE ( 'NONE', #14679, #15619 ) ;
#16672 = CARTESIAN_POINT ( 'NONE',  ( 8.343749997951613651, 2.246813503491833508, -4.409619785863906571 ) ) ;
#16673 = VERTEX_POINT ( 'NONE', #17531 ) ;
#16674 = EDGE_CURVE ( 'NONE', #9544, #12464, #6987, .T. ) ;
#16675 = CARTESIAN_POINT ( 'NONE',  ( 0.6764999999999817826, 0.000000000000000000, 0.000000000000000000 ) ) ;
#16676 = VERTEX_POINT ( 'NONE', #7286 ) ;
#16677 = DIRECTION ( 'NONE',  ( 0.000000000000000000, 0.000000000000000000, 1.000000000000000000 ) ) ;
#16678 = AXIS2_PLACEMENT_3D ( 'NONE', #10315, #17809, #14525 ) ;
#16679 = ORIENTED_EDGE ( 'NONE', *, *, #11884, .T. ) ;
#16680 = AXIS2_PLACEMENT_3D ( 'NONE', #17899, #14998, #1290 ) ;
#16681 = EDGE_CURVE ( 'NONE', #5756, #4658, #11791, .T. ) ;
#16682 = VECTOR ( 'NONE', #1011, 1000.000000000000000 ) ;
#16683 = AXIS2_PLACEMENT_3D ( 'NONE', #12700, #14004, #17106 ) ;
#16684 = CARTESIAN_POINT ( 'NONE',  ( 8.000000000000000000, 0.000000000000000000, 0.000000000000000000 ) ) ;
#16685 = DIRECTION ( 'NONE',  ( 0.000000000000000000, 0.000000000000000000, -1.000000000000000000 ) ) ;
#16686 = EDGE_CURVE ( 'NONE', #11813, #2358, #16329, .T. ) ;
#16687 = ORIENTED_EDGE ( 'NONE', *, *, #18759, .F. ) ;
#16688 = CARTESIAN_POINT ( 'NONE',  ( 0.7589665203264103210, -19.12621924769880977, 19.86422722021305631 ) ) ;
#16689 = EDGE_CURVE ( 'NONE', #17179, #2660, #19307, .T. ) ;
#16690 = DIRECTION ( 'NONE',  ( 0.000000000000000000, 0.000000000000000000, 1.000000000000000000 ) ) ;
#16691 = ORIENTED_EDGE ( 'NONE', *, *, #2097, .T. ) ;
#16692 = DIRECTION ( 'NONE',  ( 0.000000000000000000, 0.000000000000000000, 1.000000000000000000 ) ) ;
#16693 = AXIS2_PLACEMENT_3D ( 'NONE', #17099, #194, #6667 ) ;
#16694 = FACE_BOUND ( 'NONE', #19161, .T. ) ;
#16695 = AXIS2_PLACEMENT_3D ( 'NONE', #4859, #7552, #1470 ) ;
#16696 = DIRECTION ( 'NONE',  ( 0.000000000000000000, 0.000000000000000000, -1.000000000000000000 ) ) ;
#16697 = CIRCLE ( 'NONE', #81, 6.000000000000000000 ) ;
#16698 = CARTESIAN_POINT ( 'NONE',  ( 6.626241948324199882, -16.73597674598852691, 35.00000000000000000 ) ) ;
#16699 = DIRECTION ( 'NONE',  ( 1.000000000000000000, -0.000000000000000000, -0.000000000000000000 ) ) ;
#16700 = VERTEX_POINT ( 'NONE', #5795 ) ;
#16701 = LINE ( 'NONE', #281, #15719 ) ;
#16702 = CARTESIAN_POINT ( 'NONE',  ( 2.789999999999999147, -24.04302995059966719, 1.991882183130210482 ) ) ;
#16703 = EDGE_LOOP ( 'NONE', ( #15374, #15395 ) ) ;
#16704 = CARTESIAN_POINT ( 'NONE',  ( 11.81249999590322552, -2.068159791354221344, 5.387740456496221242 ) ) ;
#16705 = ADVANCED_FACE ( 'NONE', ( #5698 ), #2698, .F. ) ;
#16706 = CARTESIAN_POINT ( 'NONE',  ( -7.700916879387133607E-14, 12.51293083811828843, -20.85287692521917080 ) ) ;
#16707 = AXIS2_PLACEMENT_3D ( 'NONE', #18569, #10774, #9682 ) ;
#16708 = CIRCLE ( 'NONE', #12508, 4.400000000000000355 ) ;
#16709 = CARTESIAN_POINT ( 'NONE',  ( 0.02436607992775978102, 2.336989772644613161, -24.63872515616080250 ) ) ;
#16710 = CYLINDRICAL_SURFACE ( 'NONE', #2029, 2.524999999999995914 ) ;
#16711 = VERTEX_POINT ( 'NONE', #19709 ) ;
#16712 = ADVANCED_FACE ( 'NONE', ( #14917 ), #9115, .F. ) ;
#16713 = DIRECTION ( 'NONE',  ( 0.000000000000000000, 0.000000000000000000, 1.000000000000000000 ) ) ;
#16714 = FILL_AREA_STYLE_COLOUR ( '', #16735 ) ;
#16715 = CARTESIAN_POINT ( 'NONE',  ( -11.00000000000000355, -3.278623949159158446, -2.625000000000002220 ) ) ;
#16716 = EDGE_CURVE ( 'NONE', #5566, #4750, #9595, .T. ) ;
#16717 = AXIS2_PLACEMENT_3D ( 'NONE', #17893, #986, #8399 ) ;
#16718 = VERTEX_POINT ( 'NONE', #18315 ) ;
#16719 = DIRECTION ( 'NONE',  ( 0.000000000000000000, 0.000000000000000000, 1.000000000000000000 ) ) ;
#16720 = CARTESIAN_POINT ( 'NONE',  ( 2.718131914667133220, 10.24630254990516143, 23.19485392143217339 ) ) ;
#16721 = FACE_OUTER_BOUND ( 'NONE', #7937, .T. ) ;
#16722 = CARTESIAN_POINT ( 'NONE',  ( 9.843749997951615427, 3.954556930911862000, -2.873153789725825469 ) ) ;
#16723 = FACE_OUTER_BOUND ( 'NONE', #17163, .T. ) ;
#16724 = AXIS2_PLACEMENT_3D ( 'NONE', #17428, #9833, #6230 ) ;
#16725 = EDGE_CURVE ( 'NONE', #12283, #7096, #6051, .T. ) ;
#16726 = CARTESIAN_POINT ( 'NONE',  ( -11.58013454126452579, -14.56230589874905235, 32.00000000000000000 ) ) ;
#16727 = VERTEX_POINT ( 'NONE', #10328 ) ;
#16728 = CARTESIAN_POINT ( 'NONE',  ( -3.846120219227966430, -3.114526743279228072, -10.96874999795161720 ) ) ;
#16729 = CARTESIAN_POINT ( 'NONE',  ( 1.749999999999998002, 24.89775460606851354, -12.96210679857759729 ) ) ;
#16730 = VERTEX_POINT ( 'NONE', #4609 ) ;
#16731 = AXIS2_PLACEMENT_3D ( 'NONE', #4091, #10103, #16203 ) ;
#16732 = DIRECTION ( 'NONE',  ( -1.000000000000000000, -0.000000000000000000, -0.000000000000000000 ) ) ;
#16733 = CARTESIAN_POINT ( 'NONE',  ( 1.749999999999998002, 27.76164181293051669, -4.147968289691384314 ) ) ;
#16734 = VERTEX_POINT ( 'NONE', #18219 ) ;
#16735 = COLOUR_RGB ( '', 0.66274510, 0.83137255, 0.94901961) ;
#16736 = CYLINDRICAL_SURFACE ( 'NONE', #462, 9.000000000000021316 ) ;
#16737 = CARTESIAN_POINT ( 'NONE',  ( 10.34374999795161543, 4.150607464521792522, 2.695436003842732298 ) ) ;
#16738 = CARTESIAN_POINT ( 'NONE',  ( -3.499494075959816541, 3.499494075959816541, -8.968749997951613651 ) ) ;
#16739 = EDGE_CURVE ( 'NONE', #17554, #2370, #7997, .T. ) ;
#16740 = VERTEX_POINT ( 'NONE', #13510 ) ;
#16741 = FACE_OUTER_BOUND ( 'NONE', #9071, .T. ) ;
#16742 = ORIENTED_EDGE ( 'NONE', *, *, #14685, .F. ) ;
#16743 = CARTESIAN_POINT ( 'NONE',  ( 0.02436607992776498519, -21.30679549418621832, -12.59161484032935618 ) ) ;
#16744 = VERTEX_POINT ( 'NONE', #18028 ) ;
#16745 = CARTESIAN_POINT ( 'NONE',  ( 0.000000000000000000, 0.000000000000000000, -6.527800000000000047 ) ) ;
#16746 = AXIS2_PLACEMENT_3D ( 'NONE', #15527, #7907, #8516 ) ;
#16747 = DIRECTION ( 'NONE',  ( -0.000000000000000000, 0.000000000000000000, 1.000000000000000000 ) ) ;
#16748 = CARTESIAN_POINT ( 'NONE',  ( 0.02436607992775544421, -22.71065055754445439, -9.836394144775947979 ) ) ;
#16749 = FACE_OUTER_BOUND ( 'NONE', #5598, .T. ) ;
#16750 = CARTESIAN_POINT ( 'NONE',  ( 2.031033479673586939, 19.86422722021340093, -19.12621924769845805 ) ) ;
#16751 = ORIENTED_EDGE ( 'NONE', *, *, #527, .F. ) ;
#16752 = CARTESIAN_POINT ( 'NONE',  ( 1.039999999999997593, 0.000000000000000000, 0.000000000000000000 ) ) ;
#16753 = STYLED_ITEM ( 'NONE', ( #6166 ), #7808 ) ;
#16754 = AXIS2_PLACEMENT_3D ( 'NONE', #14249, #12257, #6228 ) ;
#16755 = ADVANCED_FACE ( 'NONE', ( #16721 ), #10421, .F. ) ;
#16756 = DIRECTION ( 'NONE',  ( -0.8660254037844419273, 0.4999999999999944489, 0.000000000000000000 ) ) ;
#16757 = EDGE_CURVE ( 'NONE', #17855, #257, #13712, .T. ) ;
#16758 = ADVANCED_FACE ( 'NONE', ( #1308 ), #7386, .F. ) ;
#16759 =( BOUNDED_CURVE ( )  B_SPLINE_CURVE ( 2, ( #8609, #19021, #14718, #5312, #13304, #19406, #11809, #17912, #4204, #10320, #16415, #2692, #15212, #9210, #1504, #7281, #12207 ),
 .UNSPECIFIED., .F., .F. ) 
 B_SPLINE_CURVE_WITH_KNOTS ( ( 3, 2, 2, 2, 2, 2, 2, 2, 3 ),
 ( 0.000000000000000000, 0.05000000000000000971, 0.1000000000000000194, 0.1499999999999999944, 0.2000000000000000389, 0.2500000000000000000, 0.2999999999999999889, 0.3499999999999999223, 0.4000000000000000777 ),
 .UNSPECIFIED. ) 
 CURVE ( )  GEOMETRIC_REPRESENTATION_ITEM ( )  RATIONAL_B_SPLINE_CURVE ( ( 1.000000000000000000, 0.9876883405951377704, 1.000000000000000000, 0.9876883405951377704, 1.000000000000000000, 0.9876883405951377704, 1.000000000000000000, 0.9876883405951377704, 1.000000000000000000, 0.9876883405951377704, 1.000000000000000000, 0.9876883405951377704, 1.000000000000000000, 0.9876883405951377704, 1.000000000000000000, 0.9876883405951377704, 1.000000000000000000 ) ) 
 REPRESENTATION_ITEM ( '' )  );
#16760 = ORIENTED_EDGE ( 'NONE', *, *, #19203, .F. ) ;
#16761 = B_SPLINE_CURVE_WITH_KNOTS ( 'NONE', 3,
 ( #9773, #11364, #6731, #18755, #2049, #8460, #13056, #16061 ),
 .UNSPECIFIED., .F., .F.,
 ( 4, 2, 2, 4 ),
 ( 2.032124546156068561E-07, 0.001631739532304432192, 0.002447507692229335726, 0.003263275852154239043 ),
 .UNSPECIFIED. ) ;
#16762 = VECTOR ( 'NONE', #1274, 1000.000000000000000 ) ;
#16763 = DIRECTION ( 'NONE',  ( 0.000000000000000000, 0.000000000000000000, 1.000000000000000000 ) ) ;
#16764 = CYLINDRICAL_SURFACE ( 'NONE', #4567, 1.000000000000003109 ) ;
#16765 = ORIENTED_EDGE ( 'NONE', *, *, #2662, .F. ) ;
#16766 = DIRECTION ( 'NONE',  ( 1.000000000000000000, 0.000000000000000000, 0.000000000000000000 ) ) ;
#16767 = LINE ( 'NONE', #1249, #5920 ) ;
#16768 = EDGE_CURVE ( 'NONE', #8931, #6178, #9754, .T. ) ;
#16769 = ADVANCED_FACE ( 'NONE', ( #301 ), #16919, .T. ) ;
#16770 = ORIENTED_EDGE ( 'NONE', *, *, #8558, .T. ) ;
#16771 = DIRECTION ( 'NONE',  ( 0.000000000000000000, 1.224646799147353207E-16, 1.000000000000000000 ) ) ;
#16772 = EDGE_LOOP ( 'NONE', ( #11714, #17386, #1967, #10587, #18125 ) ) ;
#16773 = FACE_OUTER_BOUND ( 'NONE', #16473, .T. ) ;
#16774 =( NAMED_UNIT ( * ) PLANE_ANGLE_UNIT ( ) SI_UNIT ( $, .RADIAN. ) );
#16775 = ORIENTED_EDGE ( 'NONE', *, *, #17146, .F. ) ;
#16776 = ORIENTED_EDGE ( 'NONE', *, *, #15830, .T. ) ;
#16777 = DIRECTION ( 'NONE',  ( -1.000000000000000000, -0.000000000000000000, -0.000000000000000000 ) ) ;
#16778 = CARTESIAN_POINT ( 'NONE',  ( 5.574407415329156734, -1.493657965219523209, -14.81249999590322552 ) ) ;
#16780 = ORIENTED_EDGE ( 'NONE', *, *, #12443, .T. ) ;
#16779 = AXIS2_PLACEMENT_3D ( 'NONE', #622, #1913, #18624 ) ;
#16781 = DIRECTION ( 'NONE',  ( 1.000000000000000000, 0.000000000000000000, 0.000000000000000000 ) ) ;
#16782 = VERTEX_POINT ( 'NONE', #11005 ) ;
#16783 = DIRECTION ( 'NONE',  ( -0.000000000000000000, -0.000000000000000000, 1.000000000000000000 ) ) ;
#16784 = PRODUCT_DEFINITION ( 'UNKNOWN', '', #16266, #18800 ) ;
#16785 = ORIENTED_EDGE ( 'NONE', *, *, #11138, .F. ) ;
#16786 = EDGE_CURVE ( 'NONE', #4617, #15369, #7992, .T. ) ;
#16787 = CARTESIAN_POINT ( 'NONE',  ( -41.99999999999999289, -5.000000000000001776, 5.000000000000000000 ) ) ;
#16788 = CARTESIAN_POINT ( 'NONE',  ( 12.34374999795161543, 4.888101187500000222, 0.7741991708318884946 ) ) ;
#16789 = CARTESIAN_POINT ( 'NONE',  ( 0.02436607992776368414, 18.55949924794916228, -16.37294372382838148 ) ) ;
#16790 = ADVANCED_FACE ( 'NONE', ( #14205 ), #11778, .F. ) ;
#16791 = ORIENTED_EDGE ( 'NONE', *, *, #9806, .T. ) ;
#16792 = EDGE_LOOP ( 'NONE', ( #4425, #7336, #6222, #12148 ) ) ;
#16793 = CARTESIAN_POINT ( 'NONE',  ( -11.00000000000000355, 4.898587196589412829E-16, 0.000000000000000000 ) ) ;
#16794 = CARTESIAN_POINT ( 'NONE',  ( 6.626241948324199882, -16.73597674598852691, -32.00000000000000000 ) ) ;
#16795 = ORIENTED_EDGE ( 'NONE', *, *, #3132, .F. ) ;
#16796 = CARTESIAN_POINT ( 'NONE',  ( 2.604434261026090436, 5.253342437940084153, -25.39738473784996131 ) ) ;
#16797 = CIRCLE ( 'NONE', #14234, 24.12539914357697768 ) ;
#16798 = DIRECTION ( 'NONE',  ( -1.000000000000000000, -0.000000000000000000, 0.000000000000000000 ) ) ;
#16799 = B_SPLINE_CURVE_WITH_KNOTS ( 'NONE', 3,
 ( #6999, #2503, #11715, #8226, #5319, #11432 ),
 .UNSPECIFIED., .F., .F.,
 ( 4, 2, 4 ),
 ( 2.586195665723156346E-07, 0.001878649493629684468, 0.003757040367692796902 ),
 .UNSPECIFIED. ) ;
#16800 = VECTOR ( 'NONE', #14399, 1000.000000000000000 ) ;
#16801 = DIRECTION ( 'NONE',  ( -1.000000000000000000, -0.000000000000000000, -0.000000000000000000 ) ) ;
#16802 = EDGE_CURVE ( 'NONE', #3927, #18676, #204, .T. ) ;
#16803 = CARTESIAN_POINT ( 'NONE',  ( 2.299999999999996270, 0.000000000000000000, -6.000000000000021316 ) ) ;
#16804 = CARTESIAN_POINT ( 'NONE',  ( 12.99999999999999467, 4.471046188018904743, 1.976722499206014838 ) ) ;
#16805 = ORIENTED_EDGE ( 'NONE', *, *, #17542, .T. ) ;
#16806 = CARTESIAN_POINT ( 'NONE',  ( 2.850000000000024070, 4.936344801571289409, -6.656249997951614539 ) ) ;
#16807 = LINE ( 'NONE', #10792, #5952 ) ;
#16808 = EDGE_CURVE ( 'NONE', #6045, #10924, #5445, .T. ) ;
#16809 = ORIENTED_EDGE ( 'NONE', *, *, #11170, .F. ) ;
#16810 = DIRECTION ( 'NONE',  ( -0.000000000000000000, -0.000000000000000000, 1.000000000000000000 ) ) ;
#16811 = ADVANCED_FACE ( 'NONE', ( #3889 ), #13827, .T. ) ;
#16812 = FACE_OUTER_BOUND ( 'NONE', #8280, .T. ) ;
#16813 = TOROIDAL_SURFACE ( 'NONE', #17450, 24.12539914357697768, 8.000000000000000000 ) ;
#16814 = AXIS2_PLACEMENT_3D ( 'NONE', #3056, #6714, #1832 ) ;
#16815 = CARTESIAN_POINT ( 'NONE',  ( 6.468749997951615427, -4.233219804643852946, -2.444050593750049849 ) ) ;
#16816 = CYLINDRICAL_SURFACE ( 'NONE', #3957, 2.524999999999995914 ) ;
#16817 = ORIENTED_EDGE ( 'NONE', *, *, #13612, .T. ) ;
#16818 = CARTESIAN_POINT ( 'NONE',  ( 11.00000000000000711, 5.700000000000001066, -3.490243377569957047E-16 ) ) ;
#16819 =( NAMED_UNIT ( * ) PLANE_ANGLE_UNIT ( ) SI_UNIT ( $, .RADIAN. ) );
#16820 = DIRECTION ( 'NONE',  ( 0.000000000000000000, 0.000000000000000000, 1.000000000000000000 ) ) ;
#16821 = DIRECTION ( 'NONE',  ( -1.000000000000000000, -0.000000000000000000, -0.000000000000000000 ) ) ;
#16822 = ORIENTED_EDGE ( 'NONE', *, *, #1148, .T. ) ;
#16823 = CARTESIAN_POINT ( 'NONE',  ( 5.207209108562820710, -2.318398865532073305, -14.00000000000000533 ) ) ;
#16824 = DIRECTION ( 'NONE',  ( 0.000000000000000000, -0.7315216790650488354, -0.6818181818181821008 ) ) ;
#16825 = CARTESIAN_POINT ( 'NONE',  ( 12.46874999795161543, 1.016293382781411792, 4.781284448697194378 ) ) ;
#16826 = CARTESIAN_POINT ( 'NONE',  ( 2.500000000000002220, 0.000000000000000000, 6.543750000000017941 ) ) ;
#16827 = VERTEX_POINT ( 'NONE', #6875 ) ;
#16828 = DIRECTION ( 'NONE',  ( 1.000000000000000000, 0.000000000000000000, 0.000000000000000000 ) ) ;
#16829 = CARTESIAN_POINT ( 'NONE',  ( 4.942249507334556924, 0.2590123213420975623, -13.34374999795161365 ) ) ;
#16830 = VECTOR ( 'NONE', #14731, 1000.000000000000000 ) ;
#16831 = EDGE_LOOP ( 'NONE', ( #3312, #15022, #12985, #2247 ) ) ;
#16832 = CARTESIAN_POINT ( 'NONE',  ( 6.468749997951615427, -3.413342815706642518E-14, 4.888101187500000222 ) ) ;
#16833 = CARTESIAN_POINT ( 'NONE',  ( 0.5279273381794625797, 26.82026385750178932, 3.461047254864356049 ) ) ;
#16834 = ORIENTED_EDGE ( 'NONE', *, *, #7911, .T. ) ;
#16835 = CARTESIAN_POINT ( 'NONE',  ( 5.500000000000005329, 0.000000000000000000, 0.000000000000000000 ) ) ;
#16836 = CARTESIAN_POINT ( 'NONE',  ( 2.604434325169353581, 25.77772010606605946, -2.851997810081738027 ) ) ;
#16837 = ORIENTED_EDGE ( 'NONE', *, *, #19677, .T. ) ;
#16838 = AXIS2_PLACEMENT_3D ( 'NONE', #12087, #17789, #4085 ) ;
#16839 = CARTESIAN_POINT ( 'NONE',  ( -1.900000000000000133, 8.239200000000002078, 0.000000000000000000 ) ) ;
#16840 = CARTESIAN_POINT ( 'NONE',  ( 2.000000000000000000, 4.200000000000000178, 0.000000000000000000 ) ) ;
#16841 = AXIS2_PLACEMENT_3D ( 'NONE', #4886, #9699, #17190 ) ;
#16842 = ORIENTED_EDGE ( 'NONE', *, *, #16041, .T. ) ;
#16843 = CYLINDRICAL_SURFACE ( 'NONE', #7015, 2.524999999999995914 ) ;
#16844 = ORIENTED_EDGE ( 'NONE', *, *, #11379, .F. ) ;
#16845 = CARTESIAN_POINT ( 'NONE',  ( -3.476417968967383754, 17.43449690031536292, -32.00000000000000000 ) ) ;
#16846 = EDGE_LOOP ( 'NONE', ( #12449, #4872, #2155, #5167 ) ) ;
#16847 = DIRECTION ( 'NONE',  ( -1.000000000000000000, -0.000000000000000000, 0.000000000000000000 ) ) ;
#16848 = CARTESIAN_POINT ( 'NONE',  ( 2.765633920072235963, 22.71065055754452544, 9.836394144775786330 ) ) ;
#16849 = CARTESIAN_POINT ( 'NONE',  ( -1.310841663519413114, 0.000000000000000000, 4.000000000000000000 ) ) ;
#16850 = FACE_OUTER_BOUND ( 'NONE', #18610, .T. ) ;
#16851 = CARTESIAN_POINT ( 'NONE',  ( 1.394999999999999574, -20.02152543075331081, -19.67366047555552555 ) ) ;
#16852 = EDGE_LOOP ( 'NONE', ( #11326, #15475 ) ) ;
#16853 = CARTESIAN_POINT ( 'NONE',  ( -18.11901729331277267, 5.562305898749051458, 32.00000000000000000 ) ) ;
#16854 = VECTOR ( 'NONE', #18243, 1000.000000000000000 ) ;
#16855 = ADVANCED_FACE ( 'NONE', ( #19189 ), #5481, .T. ) ;
#16856 = AXIS2_PLACEMENT_3D ( 'NONE', #15637, #9746, #4930 ) ;
#16857 = ORIENTED_EDGE ( 'NONE', *, *, #19592, .F. ) ;
#16858 = CARTESIAN_POINT ( 'NONE',  ( -11.00000000000000355, -4.215373648918917304, -3.375000000000002665 ) ) ;
#16859 = CARTESIAN_POINT ( 'NONE',  ( 112.0000000000000000, 0.000000000000000000, 0.000000000000000000 ) ) ;
#16860 = EDGE_LOOP ( 'NONE', ( #17552, #5625, #1005 ) ) ;
#16861 = CARTESIAN_POINT ( 'NONE',  ( 7.000000000000005329, -5.575441324182703440, 1.185096637661176677 ) ) ;
#16862 = CARTESIAN_POINT ( 'NONE',  ( 2.790000000000077751, 24.22524813288762147, 2.133839912090885527 ) ) ;
#16863 = VERTEX_POINT ( 'NONE', #5089 ) ;
#16864 = CARTESIAN_POINT ( 'NONE',  ( -2.444050593749990341, 4.233219804643887585, -6.468749997951615427 ) ) ;
#16865 = AXIS2_PLACEMENT_3D ( 'NONE', #19120, #5599, #3719 ) ;
#16866 = VERTEX_POINT ( 'NONE', #12905 ) ;
#16867 = SHAPE_DEFINITION_REPRESENTATION ( #767, #12077 ) ;
#16868 = CARTESIAN_POINT ( 'NONE',  ( 50.00050000000000239, 4.898587196589412829E-16, -4.000000000000000000 ) ) ;
#16869 = AXIS2_PLACEMENT_3D ( 'NONE', #8355, #1948, #6734 ) ;
#16870 = CARTESIAN_POINT ( 'NONE',  ( 0.000000000000000000, 0.000000000000000000, 0.000000000000000000 ) ) ;
#16871 = EDGE_LOOP ( 'NONE', ( #5586, #15278, #1368, #2590 ) ) ;
#16872 = EDGE_CURVE ( 'NONE', #1230, #6609, #11522, .T. ) ;
#16873 = EDGE_LOOP ( 'NONE', ( #3160, #8639, #12473, #9670 ) ) ;
#16874 = DIRECTION ( 'NONE',  ( 1.000000000000000000, -0.000000000000000000, 0.000000000000000000 ) ) ;
#16875 = CARTESIAN_POINT ( 'NONE',  ( 12.92161831991541554, 4.611601942845662272, 1.625176344145936147 ) ) ;
#16876 = ORIENTED_EDGE ( 'NONE', *, *, #9538, .T. ) ;
#16877 = EDGE_CURVE ( 'NONE', #13977, #18458, #2881, .T. ) ;
#16878 = DIRECTION ( 'NONE',  ( -1.000000000000000000, 0.000000000000000000, 0.000000000000000000 ) ) ;
#16879 = VECTOR ( 'NONE', #14893, 1000.000000000000000 ) ;
#16880 = EDGE_LOOP ( 'NONE', ( #19090, #15234, #6812, #17745 ) ) ;
#16881 = VECTOR ( 'NONE', #6197, 1000.000000000000000 ) ;
#16882 = DIRECTION ( 'NONE',  ( -1.000000000000000000, 0.000000000000000000, 0.000000000000000000 ) ) ;
#16883 = DIRECTION ( 'NONE',  ( -1.000000000000000000, -0.000000000000000000, -0.000000000000000000 ) ) ;
#16884 = DIRECTION ( 'NONE',  ( -0.000000000000000000, -0.000000000000000000, -1.000000000000000000 ) ) ;
#16885 = ORIENTED_EDGE ( 'NONE', *, *, #13076, .T. ) ;
#16886 = ORIENTED_EDGE ( 'NONE', *, *, #914, .F. ) ;
#16887 = DIRECTION ( 'NONE',  ( -1.000000000000000000, -0.000000000000000000, -0.000000000000000000 ) ) ;
#16888 =( NAMED_UNIT ( * ) SI_UNIT ( $, .STERADIAN. ) SOLID_ANGLE_UNIT ( ) );
#16889 = CARTESIAN_POINT ( 'NONE',  ( 2.789999999999999147, -7.909232158574647009, -21.81711360614308148 ) ) ;
#16890 = ORIENTED_EDGE ( 'NONE', *, *, #19319, .T. ) ;
#16891 = EDGE_CURVE ( 'NONE', #10624, #4466, #11203, .T. ) ;
#16892 = ORIENTED_EDGE ( 'NONE', *, *, #1920, .T. ) ;
#16893 = FACE_OUTER_BOUND ( 'NONE', #1223, .T. ) ;
#16894 = DIRECTION ( 'NONE',  ( 1.000000000000000000, 0.000000000000000000, -0.000000000000000000 ) ) ;
#16895 = DIRECTION ( 'NONE',  ( 0.000000000000000000, 0.000000000000000000, -1.000000000000000000 ) ) ;
#16896 = CARTESIAN_POINT ( 'NONE',  ( 1.960886852992457241, 24.44424927289185945, 12.96989951879416125 ) ) ;
#16897 = EDGE_CURVE ( 'NONE', #11950, #12571, #5189, .T. ) ;
#16898 = CARTESIAN_POINT ( 'NONE',  ( -5.699999999999999289, 0.9027913098498568933, -6.500000000000005329 ) ) ;
#16899 = ORIENTED_EDGE ( 'NONE', *, *, #7729, .F. ) ;
#16900 = DIRECTION ( 'NONE',  ( 1.000000000000000000, 0.000000000000000000, 0.000000000000000000 ) ) ;
#16901 = EDGE_CURVE ( 'NONE', #10556, #3868, #6781, .T. ) ;
#16902 = CARTESIAN_POINT ( 'NONE',  ( 0.8291131470075020493, -24.44424927289185590, 12.96989951879399072 ) ) ;
#16903 =( REPRESENTATION_RELATIONSHIP ('NONE','NONE', #18211, #7967 ) REPRESENTATION_RELATIONSHIP_WITH_TRANSFORMATION ( #5243 )SHAPE_REPRESENTATION_RELATIONSHIP( ) );
#16904 = ORIENTED_EDGE ( 'NONE', *, *, #19561, .T. ) ;
#16905 = CARTESIAN_POINT ( 'NONE',  ( 0.000000000000000000, 0.000000000000000000, -22.00000000000000000 ) ) ;
#16906 = CARTESIAN_POINT ( 'NONE',  ( 0.000000000000000000, 0.000000000000000000, -28.99999999999999645 ) ) ;
#16907 = AXIS2_PLACEMENT_3D ( 'NONE', #854, #5141, #11257 ) ;
#16908 = CARTESIAN_POINT ( 'NONE',  ( -2.850000000000058265, -4.936344801571268093, -7.312499995903225525 ) ) ;
#16909 = CARTESIAN_POINT ( 'NONE',  ( 0.006974657972266581039, -23.92335783895634194, -5.408388659524344000 ) ) ;
#16910 = EDGE_CURVE ( 'NONE', #1803, #7371, #17504, .T. ) ;
#16911 = ORIENTED_EDGE ( 'NONE', *, *, #11981, .T. ) ;
#16912 = CARTESIAN_POINT ( 'NONE',  ( 6.500000000000005329, 0.9027913098498568933, -5.699999999999999289 ) ) ;
#16913 = DIRECTION ( 'NONE',  ( -1.000000000000000000, -0.000000000000000000, -0.000000000000000000 ) ) ;
#16914 = DIRECTION ( 'NONE',  ( 0.000000000000000000, 0.000000000000000000, -1.000000000000000000 ) ) ;
#16915 = ORIENTED_EDGE ( 'NONE', *, *, #1660, .F. ) ;
#16916 = DIRECTION ( 'NONE',  ( 0.8660254037844383745, 0.5000000000000004441, 0.000000000000000000 ) ) ;
#16917 = CARTESIAN_POINT ( 'NONE',  ( 12.46874999795161543, -3.632567103900546712, 3.270778111535314281 ) ) ;
#16918 = EDGE_CURVE ( 'NONE', #14843, #16727, #9940, .T. ) ;
#16919 = PLANE ( 'NONE',  #4807 ) ;
#16920 = EDGE_CURVE ( 'NONE', #4658, #12853, #2875, .T. ) ;
#16921 = CARTESIAN_POINT ( 'NONE',  ( 2.444050593749960587, -4.233219804643904460, -6.468749997951615427 ) ) ;
#16922 = ORIENTED_EDGE ( 'NONE', *, *, #2107, .F. ) ;
#16923 = CARTESIAN_POINT ( 'NONE',  ( 0.5279272304333949561, 11.57956866523252870, -24.43806413951663004 ) ) ;
#16924 = CIRCLE ( 'NONE', #15966, 1.000000000000004441 ) ;
#16925 = LINE ( 'NONE', #8204, #13676 ) ;
#16926 = VERTEX_POINT ( 'NONE', #5969 ) ;
#16927 = CARTESIAN_POINT ( 'NONE',  ( 7.968749997951616315, -2.246813503491864150, 4.409619785863891472 ) ) ;
#16928 = DIRECTION ( 'NONE',  ( -1.000000000000000000, 0.000000000000000000, -0.000000000000000000 ) ) ;
#16929 = COLOUR_RGB ( '', 0.09019608, 0.27058824, 0.51372549) ;
#16930 = ORIENTED_EDGE ( 'NONE', *, *, #2521, .T. ) ;
#16931 = EDGE_CURVE ( 'NONE', #7032, #9186, #15191, .T. ) ;
#16932 = ADVANCED_FACE ( 'NONE', ( #11793 ), #5579, .F. ) ;
#16933 = CARTESIAN_POINT ( 'NONE',  ( 2.246813503491833508, 4.409619785863906571, -13.34374999795161365 ) ) ;
#16934 = CARTESIAN_POINT ( 'NONE',  ( 2.246813503491803310, -4.409619785863921670, -10.34374999795161543 ) ) ;
#16935 = ORIENTED_EDGE ( 'NONE', *, *, #13962, .T. ) ;
#16936 = CARTESIAN_POINT ( 'NONE',  ( -2.000000000000001776, 0.000000000000000000, 0.000000000000000000 ) ) ;
#16937 = ORIENTED_EDGE ( 'NONE', *, *, #7117, .T. ) ;
#16938 = DIRECTION ( 'NONE',  ( -1.000000000000000000, -0.000000000000000000, -0.000000000000000000 ) ) ;
#16939 = VERTEX_POINT ( 'NONE', #19588 ) ;
#16940 = EDGE_CURVE ( 'NONE', #9700, #19560, #14798, .T. ) ;
#16941 = CARTESIAN_POINT ( 'NONE',  ( 0.000000000000000000, 20.70663861606272249, 15.04425356660767932 ) ) ;
#16942 = ORIENTED_EDGE ( 'NONE', *, *, #6650, .F. ) ;
#16943 = AXIS2_PLACEMENT_3D ( 'NONE', #13837, #2024, #9440 ) ;
#16944 = VECTOR ( 'NONE', #1822, 1000.000000000000000 ) ;
#16945 = DIRECTION ( 'NONE',  ( 0.000000000000000000, 0.000000000000000000, 1.000000000000000000 ) ) ;
#16946 = DIRECTION ( 'NONE',  ( -0.8090169943749481174, -0.5877852522924720269, 0.000000000000000000 ) ) ;
#16947 = DIRECTION ( 'NONE',  ( -1.000000000000000000, 0.000000000000000000, 0.000000000000000000 ) ) ;
#16948 = CARTESIAN_POINT ( 'NONE',  ( 12.99999999999999467, 0.3329550909587259966, 4.877148943244128176 ) ) ;
#16949 = ORIENTED_EDGE ( 'NONE', *, *, #18082, .F. ) ;
#16950 = CYLINDRICAL_SURFACE ( 'NONE', #13498, 13.20000000000000284 ) ;
#16951 = CARTESIAN_POINT ( 'NONE',  ( -34.92499999999994742, 0.000000000000000000, 0.000000000000000000 ) ) ;
#16952 = AXIS2_PLACEMENT_3D ( 'NONE', #11889, #1286, #18197 ) ;
#16953 = VERTEX_POINT ( 'NONE', #5876 ) ;
#16954 = AXIS2_PLACEMENT_3D ( 'NONE', #797, #8765, #5744 ) ;
#16955 = DIRECTION ( 'NONE',  ( -0.000000000000000000, -0.000000000000000000, 1.000000000000000000 ) ) ;
#16956 = CARTESIAN_POINT ( 'NONE',  ( 2.765633920072236851, -22.71065055754445439, -9.836394144775947979 ) ) ;
#16957 = EDGE_LOOP ( 'NONE', ( #13656, #14438, #15154, #12332, #5536, #9077 ) ) ;
#16958 = FACE_OUTER_BOUND ( 'NONE', #12902, .T. ) ;
#16959 = CARTESIAN_POINT ( 'NONE',  ( 12.31249999590322552, 2.850000000000057820, -4.936344801571268093 ) ) ;
#16960 = ORIENTED_EDGE ( 'NONE', *, *, #13305, .T. ) ;
#16961 = PLANE ( 'NONE',  #5565 ) ;
#16962 = ORIENTED_EDGE ( 'NONE', *, *, #650, .F. ) ;
#16963 = SHAPE_DEFINITION_REPRESENTATION ( #11465, #17568 ) ;
#16964 = CYLINDRICAL_SURFACE ( 'NONE', #19572, 5.700000000000001954 ) ;
#16965 = EDGE_CURVE ( 'NONE', #3823, #2901, #19484, .T. ) ;
#16966 = CARTESIAN_POINT ( 'NONE',  ( 8.468749997951615427, 4.861323657744407001, 0.5109457054261784537 ) ) ;
#16967 = ORIENTED_EDGE ( 'NONE', *, *, #15770, .T. ) ;
#16968 = VERTEX_POINT ( 'NONE', #1484 ) ;
#16969 = DIRECTION ( 'NONE',  ( 1.000000000000000000, 0.000000000000000000, 0.000000000000000000 ) ) ;
#16970 = CIRCLE ( 'NONE', #1947, 8.073750000000021743 ) ;
#16971 = CARTESIAN_POINT ( 'NONE',  ( 3.846120219227944670, 3.114526743279256493, -11.34374999795161543 ) ) ;
#16972 = PRESENTATION_LAYER_ASSIGNMENT (  '', '', ( #11802 ) ) ;
#16973 = ORIENTED_EDGE ( 'NONE', *, *, #3959, .F. ) ;
#16974 = EDGE_CURVE ( 'NONE', #3279, #12070, #973, .T. ) ;
#16975 = DIRECTION ( 'NONE',  ( 0.000000000000000000, 0.000000000000000000, 1.000000000000000000 ) ) ;
#16976 = ORIENTED_EDGE ( 'NONE', *, *, #7596, .T. ) ;
#16977 = CIRCLE ( 'NONE', #17617, 28.06981291497571362 ) ;
#16978 = DIRECTION ( 'NONE',  ( 1.000000000000000000, 0.000000000000000000, 0.000000000000000000 ) ) ;
#16979 = DIRECTION ( 'NONE',  ( 0.000000000000000000, 0.000000000000000000, -1.000000000000000000 ) ) ;
#16980 = LINE ( 'NONE', #648, #3641 ) ;
#16981 = FACE_BOUND ( 'NONE', #10361, .T. ) ;
#16982 = VERTEX_POINT ( 'NONE', #8989 ) ;
#16983 = APPLICATION_CONTEXT ( 'automotive_design' ) ;
#16984 = CARTESIAN_POINT ( 'NONE',  ( -8.671566133830875600, 15.77352024078954429, 35.00000000000000000 ) ) ;
#16985 = DIRECTION ( 'NONE',  ( 0.000000000000000000, 0.000000000000000000, 1.000000000000000000 ) ) ;
#16986 = ADVANCED_FACE ( 'NONE', ( #1089 ), #13588, .F. ) ;
#16987 = ORIENTED_EDGE ( 'NONE', *, *, #11494, .F. ) ;
#16988 = ORIENTED_EDGE ( 'NONE', *, *, #7480, .F. ) ;
#16989 = CARTESIAN_POINT ( 'NONE',  ( -2.000000000000000000, 4.999999999999998224, 37.99999999999999289 ) ) ;
#16990 = CARTESIAN_POINT ( 'NONE',  ( -5.668774803599153422, 0.5958122406256767256, -14.31249999590322552 ) ) ;
#16991 = FACE_OUTER_BOUND ( 'NONE', #16368, .T. ) ;
#16992 = CARTESIAN_POINT ( 'NONE',  ( 2.430066721642811345, 23.15620303736532293, 12.90954937922509238 ) ) ;
#16993 = CIRCLE ( 'NONE', #7377, 4.400000000000000355 ) ;
#16994 = CARTESIAN_POINT ( 'NONE',  ( -4.648860486681953397, 1.510506337161861445, -7.468749997951615427 ) ) ;
#16995 = ORIENTED_EDGE ( 'NONE', *, *, #7190, .T. ) ;
#16996 = CARTESIAN_POINT ( 'NONE',  ( 3.968750000000007994, 6.874076642538976323, 0.000000000000000000 ) ) ;
#16997 = VECTOR ( 'NONE', #11816, 1000.000000000000000 ) ;
#16998 = CARTESIAN_POINT ( 'NONE',  ( -20.63749999999999574, 0.000000000000000000, 0.000000000000000000 ) ) ;
#16999 = ORIENTED_EDGE ( 'NONE', *, *, #12830, .F. ) ;
#17000 = CARTESIAN_POINT ( 'NONE',  ( 12.00000000000000533, 4.235925505221192822, -3.814044456245444081 ) ) ;
#17001 = EDGE_CURVE ( 'NONE', #9729, #15416, #17796, .T. ) ;
#17002 = ADVANCED_FACE ( 'NONE', ( #11691 ), #10400, .F. ) ;
#17003 = CARTESIAN_POINT ( 'NONE',  ( 10.84374999795161543, -3.632567103900500971, -3.270778111535363131 ) ) ;
#17004 = CARTESIAN_POINT ( 'NONE',  ( 17.11901729331276556, 5.562305898749055011, 35.00000000000000000 ) ) ;
#17005 = DIRECTION ( 'NONE',  ( 0.000000000000000000, 0.000000000000000000, 1.000000000000000000 ) ) ;
#17006 = EDGE_LOOP ( 'NONE', ( #459, #11199, #13665, #1124 ) ) ;
#17007 = AXIS2_PLACEMENT_3D ( 'NONE', #19299, #5590, #4006 ) ;
#17008 = CIRCLE ( 'NONE', #16695, 1.000000000000000888 ) ;
#17009 = CARTESIAN_POINT ( 'NONE',  ( -17.96448111170888851, 1.130229351527647585, 32.00000000000000000 ) ) ;
#17010 = LINE ( 'NONE', #15509, #3664 ) ;
#17011 = VECTOR ( 'NONE', #13889, 1000.000000000000114 ) ;
#17012 = EDGE_LOOP ( 'NONE', ( #2671, #417 ) ) ;
#17013 = DIRECTION ( 'NONE',  ( 0.000000000000000000, 0.000000000000000000, 1.000000000000000000 ) ) ;
#17014 = CARTESIAN_POINT ( 'NONE',  ( 8.468749997951615427, 4.861323657744407001, 0.5109457054261784537 ) ) ;
#17015 = DIRECTION ( 'NONE',  ( 1.000000000000000000, 6.419766481290786633E-33, -0.000000000000000000 ) ) ;
#17016 = VERTEX_POINT ( 'NONE', #19687 ) ;
#17017 = CYLINDRICAL_SURFACE ( 'NONE', #15409, 3.000000000000000000 ) ;
#17018 = CARTESIAN_POINT ( 'NONE',  ( -4.611396867937224364, -3.350375938067065906, -14.00000000000000533 ) ) ;
#17019 = EDGE_LOOP ( 'NONE', ( #19343, #3769, #843, #1870, #9840, #3442, #19491, #644 ) ) ;
#17020 = CARTESIAN_POINT ( 'NONE',  ( 6.500000000000005329, -4.484949146646330931, -3.631840208645857437 ) ) ;
#17021 = CARTESIAN_POINT ( 'NONE',  ( 2.783025325906566927, -2.249040938978666748, 24.42374957165204563 ) ) ;
#17022 = AXIS2_PLACEMENT_3D ( 'NONE', #956, #5453, #11563 ) ;
#17023 = EDGE_LOOP ( 'NONE', ( #9437, #18859, #17876 ) ) ;
#17024 = CIRCLE ( 'NONE', #19564, 0.1999999999999996503 ) ;
#17025 = CIRCLE ( 'NONE', #1700, 6.000000000000000000 ) ;
#17026 = CIRCLE ( 'NONE', #8055, 1.000000000000002665 ) ;
#17027 = DIRECTION ( 'NONE',  ( -0.9238795325112865164, -0.3826834323650906700, 0.000000000000000000 ) ) ;
#17028 = CARTESIAN_POINT ( 'NONE',  ( 1.823865745262398308, 24.74813374239829145, 12.96725027898200899 ) ) ;
#17029 = ORIENTED_EDGE ( 'NONE', *, *, #7104, .T. ) ;
#17030 = DIRECTION ( 'NONE',  ( 1.000000000000000000, 0.000000000000000000, 0.000000000000000000 ) ) ;
#17031 = CARTESIAN_POINT ( 'NONE',  ( 0.000000000000000000, 0.000000000000000000, 35.00000000000000000 ) ) ;
#17032 = EDGE_CURVE ( 'NONE', #7744, #11459, #9277, .T. ) ;
#17033 = ORIENTED_EDGE ( 'NONE', *, *, #13590, .T. ) ;
#17034 = CARTESIAN_POINT ( 'NONE',  ( 2.789999999999999147, 15.04425356660790136, -20.70663861606255196 ) ) ;
#17035 = ORIENTED_EDGE ( 'NONE', *, *, #5034, .F. ) ;
#17036 = EDGE_CURVE ( 'NONE', #3939, #155, #15989, .T. ) ;
#17037 = DIRECTION ( 'NONE',  ( 1.000000000000000000, 0.000000000000000000, 0.000000000000000000 ) ) ;
#17038 = AXIS2_PLACEMENT_3D ( 'NONE', #18166, #2843, #18259 ) ;
#17039 = VERTEX_POINT ( 'NONE', #5676 ) ;
#17040 = FACE_OUTER_BOUND ( 'NONE', #9563, .T. ) ;
#17041 = CARTESIAN_POINT ( 'NONE',  ( -4.861323657744403448, 0.5109457054262118714, -13.84374999795161543 ) ) ;
#17042 = CARTESIAN_POINT ( 'NONE',  ( 3.632567103900546712, 3.270778111535313837, -7.468749997951615427 ) ) ;
#17043 = VECTOR ( 'NONE', #16626, 1000.000000000000000 ) ;
#17044 = CARTESIAN_POINT ( 'NONE',  ( 2.695436003842704764, -4.150607464521812062, -12.96874999795161543 ) ) ;
#17045 = EDGE_CURVE ( 'NONE', #19526, #4220, #2831, .T. ) ;
#17046 = VERTEX_POINT ( 'NONE', #16498 ) ;
#17047 = CIRCLE ( 'NONE', #16717, 0.1999999999999996503 ) ;
#17048 = FACE_OUTER_BOUND ( 'NONE', #14368, .T. ) ;
#17049 =( BOUNDED_CURVE ( )  B_SPLINE_CURVE ( 2, ( #16815, #4396, #13797, #3089, #94, #19495, #16606, #12304, #4491, #18401, #2887, #5783, #18015, #4298, #2787 ),
 .UNSPECIFIED., .F., .F. ) 
 B_SPLINE_CURVE_WITH_KNOTS ( ( 3, 2, 2, 2, 2, 2, 2, 3 ),
 ( 0.000000000000000000, 0.05000000000000000278, 0.1000000000000000056, 0.1499999999999999944, 0.2000000000000000111, 0.2500000000000000000, 0.2999999999999999889, 0.3265529187307101844 ),
 .UNSPECIFIED. ) 
 CURVE ( )  GEOMETRIC_REPRESENTATION_ITEM ( )  RATIONAL_B_SPLINE_CURVE ( ( 1.000000000000000000, 0.9876883405951377704, 1.000000000000000000, 0.9876883405951377704, 1.000000000000000000, 0.9876883405951377704, 1.000000000000000000, 0.9876883405951377704, 1.000000000000000000, 0.9876883405951377704, 1.000000000000000000, 0.9876883405951377704, 1.000000000000000000, 0.9934617901676502383, 0.9938679225082089896 ) ) 
 REPRESENTATION_ITEM ( '' )  );
#17050 = CARTESIAN_POINT ( 'NONE',  ( 16.11901729331276556, 5.562305898749055011, 32.00000000000000000 ) ) ;
#17051 = STYLED_ITEM ( 'NONE', ( #2086 ), #9489 ) ;
#17052 = ORIENTED_EDGE ( 'NONE', *, *, #13095, .T. ) ;
#17053 = EDGE_CURVE ( 'NONE', #8931, #736, #2774, .T. ) ;
#17054 = DIRECTION ( 'NONE',  ( 1.000000000000000000, 0.000000000000000000, 0.000000000000000000 ) ) ;
#17055 = LINE ( 'NONE', #8028, #6469 ) ;
#17056 = VERTEX_POINT ( 'NONE', #18483 ) ;
#17057 = CARTESIAN_POINT ( 'NONE',  ( -15.19790265903627180, 9.644882309621941374, 32.00000000000000000 ) ) ;
#17058 = CARTESIAN_POINT ( 'NONE',  ( 10.84374999795161543, 1.016293382781477961, -4.781284448697179279 ) ) ;
#17059 = VECTOR ( 'NONE', #13111, 1000.000000000000000 ) ;
#17060 = ORIENTED_EDGE ( 'NONE', *, *, #17638, .F. ) ;
#17061 = CARTESIAN_POINT ( 'NONE',  ( -7.626241948324210540, -16.73597674598852336, 32.00000000000000000 ) ) ;
#17062 = ORIENTED_EDGE ( 'NONE', *, *, #591, .F. ) ;
#17063 = APPLICATION_PROTOCOL_DEFINITION ( 'draft international standard', 'automotive_design', 1998, #19395 ) ;
#17064 = CARTESIAN_POINT ( 'NONE',  ( -3.814044456245531567, -4.235925505221111997, -10.00000000000000533 ) ) ;
#17065 = CYLINDRICAL_SURFACE ( 'NONE', #15003, 13.19999999999999929 ) ;
#17066 = ORIENTED_EDGE ( 'NONE', *, *, #12990, .T. ) ;
#17067 = VERTEX_POINT ( 'NONE', #4681 ) ;
#17068 = DIRECTION ( 'NONE',  ( 1.000000000000000000, 0.000000000000000000, 0.000000000000000000 ) ) ;
#17069 = CARTESIAN_POINT ( 'NONE',  ( 2.789999999999999147, 7.909232158575156824, -21.81711360614291806 ) ) ;
#17070 = EDGE_LOOP ( 'NONE', ( #17271, #7199, #14199, #11848 ) ) ;
#17071 = EDGE_CURVE ( 'NONE', #5740, #9896, #2550, .T. ) ;
#17072 = CARTESIAN_POINT ( 'NONE',  ( 0.000000000000000000, 0.000000000000000000, -6.000000000000005329 ) ) ;
#17073 = VECTOR ( 'NONE', #10827, 1000.000000000000000 ) ;
#17074 = EDGE_CURVE ( 'NONE', #12346, #14758, #9389, .T. ) ;
#17075 = ORIENTED_EDGE ( 'NONE', *, *, #12401, .T. ) ;
#17076 = CARTESIAN_POINT ( 'NONE',  ( -5.700000000000000178, -2.180340287075187351E-16, -12.66727757604271076 ) ) ;
#17077 = FACE_OUTER_BOUND ( 'NONE', #17457, .T. ) ;
#17078 = FACE_BOUND ( 'NONE', #2846, .T. ) ;
#17079 = VERTEX_POINT ( 'NONE', #6171 ) ;
#17080 = CARTESIAN_POINT ( 'NONE',  ( 10.58013454126452046, -14.56230589874905412, 32.00000000000000000 ) ) ;
#17081 = PRESENTATION_STYLE_ASSIGNMENT (( #18873 ) ) ;
#17082 = DIRECTION ( 'NONE',  ( -1.000000000000000000, 0.000000000000000000, 0.000000000000000000 ) ) ;
#17083 = ORIENTED_EDGE ( 'NONE', *, *, #19029, .T. ) ;
#17084 = ORIENTED_EDGE ( 'NONE', *, *, #6063, .T. ) ;
#17085 = DIRECTION ( 'NONE',  ( -1.000000000000000000, -0.000000000000000000, -0.000000000000000000 ) ) ;
#17086 = CARTESIAN_POINT ( 'NONE',  ( -7.816002369513581784E-14, 15.96555658743763217, 18.34439787333512939 ) ) ;
#17087 = CARTESIAN_POINT ( 'NONE',  ( -14.86923836996421144, -11.47363181547641275, 32.00000000000000000 ) ) ;
#17088 = EDGE_CURVE ( 'NONE', #15498, #7633, #15031, .T. ) ;
#17089 = LINE ( 'NONE', #5971, #11267 ) ;
#17090 = AXIS2_PLACEMENT_3D ( 'NONE', #14418, #11415, #16214 ) ;
#17091 = CARTESIAN_POINT ( 'NONE',  ( -4.465502636338051445, -1.988169868018530462, -8.843749997951615427 ) ) ;
#17092 = ORIENTED_EDGE ( 'NONE', *, *, #7099, .F. ) ;
#17093 = DIRECTION ( 'NONE',  ( -1.000000000000000000, -0.000000000000000000, -0.000000000000000000 ) ) ;
#17094 = CARTESIAN_POINT ( 'NONE',  ( 10.84374999795161543, -4.648860486681964055, 1.510506337161829027 ) ) ;
#17095 = ORIENTED_EDGE ( 'NONE', *, *, #9879, .T. ) ;
#17096 = CARTESIAN_POINT ( 'NONE',  ( 9.000000000000005329, -0.5958122406255588199, -5.668774803599165857 ) ) ;
#17097 = EDGE_CURVE ( 'NONE', #9357, #18458, #8321, .T. ) ;
#17098 = DIRECTION ( 'NONE',  ( -0.000000000000000000, -0.000000000000000000, 1.000000000000000000 ) ) ;
#17099 = CARTESIAN_POINT ( 'NONE',  ( 2.789999999999999147, -14.18181402625728360, -19.91106274590529068 ) ) ;
#17100 = DIRECTION ( 'NONE',  ( -0.4330127018922284576, -0.7499999999999961142, 0.4999999999999977240 ) ) ;
#17101 = CARTESIAN_POINT ( 'NONE',  ( 1.510506337161829027, -4.648860486681964055, -10.46874999795161720 ) ) ;
#17102 = VERTEX_POINT ( 'NONE', #9287 ) ;
#17103 = AXIS2_PLACEMENT_3D ( 'NONE', #16905, #16810, #4981 ) ;
#17104 = DIRECTION ( 'NONE',  ( -1.000000000000000000, 0.000000000000000000, 0.000000000000000000 ) ) ;
#17105 = AXIS2_PLACEMENT_3D ( 'NONE', #16490, #2866, #10391 ) ;
#17106 = DIRECTION ( 'NONE',  ( 0.000000000000000000, 0.000000000000000000, 1.000000000000000000 ) ) ;
#17107 =( NAMED_UNIT ( * ) PLANE_ANGLE_UNIT ( ) SI_UNIT ( $, .RADIAN. ) );
#17108 = ORIENTED_EDGE ( 'NONE', *, *, #8182, .F. ) ;
#17109 = DIRECTION ( 'NONE',  ( -0.000000000000000000, -0.7315216790650492795, -0.6818181818181815457 ) ) ;
#17110 = CARTESIAN_POINT ( 'NONE',  ( 1.749999999999998002, 12.52377138324224148, 25.12109765559658570 ) ) ;
#17111 = CARTESIAN_POINT ( 'NONE',  ( 5.700000000000001954, -0.5990941410143687529, -9.668198987696284163 ) ) ;
#17112 = CARTESIAN_POINT ( 'NONE',  ( 4.424224194511527805E-17, 20.65025570340106853, -12.51972505884970488 ) ) ;
#17113 = ADVANCED_FACE ( 'NONE', ( #16991 ), #18862, .T. ) ;
#17114 = VERTEX_POINT ( 'NONE', #4582 ) ;
#17115 = CARTESIAN_POINT ( 'NONE',  ( 0.000000000000000000, 0.000000000000000000, -25.03750572909317285 ) ) ;
#17116 = B_SPLINE_CURVE_WITH_KNOTS ( 'NONE', 3,
 ( #19602, #5983, #8805, #4695, #19699, #16510 ),
 .UNSPECIFIED., .F., .F.,
 ( 4, 2, 4 ),
 ( 0.01281224986012821296, 0.01513166665602954861, 0.01745108345193088425 ),
 .UNSPECIFIED. ) ;
#17117 = CARTESIAN_POINT ( 'NONE',  ( 18.96448111170889206, 1.130229351527639370, -35.00000000000000000 ) ) ;
#17118 = ORIENTED_EDGE ( 'NONE', *, *, #5034, .T. ) ;
#17119 = CARTESIAN_POINT ( 'NONE',  ( 7.500000000000005329, -3.143139765844555900, -4.840010801796527318 ) ) ;
#17120 = CARTESIAN_POINT ( 'NONE',  ( 2.000000000000001776, 0.000000000000000000, 0.000000000000000000 ) ) ;
#17121 = AXIS2_PLACEMENT_3D ( 'NONE', #12539, #13739, #12344 ) ;
#17122 = ORIENTED_EDGE ( 'NONE', *, *, #8478, .F. ) ;
#17123 = ADVANCED_FACE ( 'NONE', ( #12292 ), #18388, .T. ) ;
#17124 = AXIS2_PLACEMENT_3D ( 'NONE', #8330, #18838, #15277 ) ;
#17125 = DIRECTION ( 'NONE',  ( -1.000000000000000000, 0.000000000000000000, -0.000000000000000000 ) ) ;
#17126 = CARTESIAN_POINT ( 'NONE',  ( 10.50000000000000533, -2.068159791354220900, 5.387740456496221242 ) ) ;
#17127 = ORIENTED_EDGE ( 'NONE', *, *, #19594, .F. ) ;
#17128 = CARTESIAN_POINT ( 'NONE',  ( -7.928732286808572430E-16, 18.34424029220111052, 15.96500990068130577 ) ) ;
#17129 = CYLINDRICAL_SURFACE ( 'NONE', #11011, 4.400000000000000355 ) ;
#17130 = VERTEX_POINT ( 'NONE', #3076 ) ;
#17131 = DIRECTION ( 'NONE',  ( -1.000000000000000000, 0.000000000000000000, 0.000000000000000000 ) ) ;
#17132 = EDGE_LOOP ( 'NONE', ( #18058, #5456, #9580, #13393 ) ) ;
#17133 = DIRECTION ( 'NONE',  ( 0.000000000000000000, 0.000000000000000000, 1.000000000000000000 ) ) ;
#17134 = VERTEX_POINT ( 'NONE', #1875 ) ;
#17135 = FACE_OUTER_BOUND ( 'NONE', #10350, .T. ) ;
#17136 = CIRCLE ( 'NONE', #13618, 6.000000000000000000 ) ;
#17137 = CARTESIAN_POINT ( 'NONE',  ( 0.07181525480391388883, 12.74223776959231991, -21.92234060054331479 ) ) ;
#17138 = EDGE_CURVE ( 'NONE', #17079, #5861, #4885, .T. ) ;
#17139 = CARTESIAN_POINT ( 'NONE',  ( -4.235925505221191933, -3.814044456245443193, -7.000000000000005329 ) ) ;
#17140 = CARTESIAN_POINT ( 'NONE',  ( 8.000000000000000000, 0.000000000000000000, 0.000000000000000000 ) ) ;
#17141 = ORIENTED_EDGE ( 'NONE', *, *, #17053, .T. ) ;
#17142 = CYLINDRICAL_SURFACE ( 'NONE', #19206, 5.200000000000000178 ) ;
#17143 = CARTESIAN_POINT ( 'NONE',  ( 13.00000000000000178, -4.568735188514048140, -1.737869959597788672 ) ) ;
#17144 = EDGE_CURVE ( 'NONE', #11459, #6633, #15390, .T. ) ;
#17145 = ORIENTED_EDGE ( 'NONE', *, *, #15895, .F. ) ;
#17146 = EDGE_CURVE ( 'NONE', #3827, #9061, #10982, .T. ) ;
#17147 = VECTOR ( 'NONE', #11683, 1000.000000000000000 ) ;
#17148 = CARTESIAN_POINT ( 'NONE',  ( 17.11901729331276556, 5.562305898749055011, -32.00000000000000000 ) ) ;
#17149 = AXIS2_PLACEMENT_3D ( 'NONE', #1881, #12591, #12688 ) ;
#17150 = CARTESIAN_POINT ( 'NONE',  ( -36.00000000000000000, 1.224646799147351975E-16, 0.000000000000000000 ) ) ;
#17151 = DIRECTION ( 'NONE',  ( 1.000000000000000000, 1.224646799147353207E-16, -0.000000000000000000 ) ) ;
#17152 = VERTEX_POINT ( 'NONE', #17087 ) ;
#17153 = DIRECTION ( 'NONE',  ( 0.000000000000000000, 0.000000000000000000, 1.000000000000000000 ) ) ;
#17154 = CARTESIAN_POINT ( 'NONE',  ( 9.312499995903225525, -2.318398865532001363, -5.207209108562852684 ) ) ;
#17155 = EDGE_LOOP ( 'NONE', ( #3243, #6729, #2855, #12717 ) ) ;
#17156 = EDGE_CURVE ( 'NONE', #16926, #4917, #13888, .T. ) ;
#17157 = DIRECTION ( 'NONE',  ( 1.000000000000000000, 0.000000000000000000, 0.000000000000000000 ) ) ;
#17158 = ORIENTED_EDGE ( 'NONE', *, *, #12124, .F. ) ;
#17159 = SHAPE_DEFINITION_REPRESENTATION ( #2353, #19604 ) ;
#17160 = CARTESIAN_POINT ( 'NONE',  ( -5.668774803599153422, 0.5958122406256767256, -13.00000000000000533 ) ) ;
#17161 = CARTESIAN_POINT ( 'NONE',  ( 13.84374999795161543, -0.5109457054261780096, 4.861323657744406113 ) ) ;
#17162 = B_SPLINE_CURVE_WITH_KNOTS ( 'NONE', 3,
 ( #9917, #12616, #9721, #15809 ),
 .UNSPECIFIED., .F., .F.,
 ( 4, 4 ),
 ( 1.981826382900847290E-07, 0.0006887856082032348722 ),
 .UNSPECIFIED. ) ;
#17163 = EDGE_LOOP ( 'NONE', ( #8671, #16805, #4202, #1182 ) ) ;
#17164 =( BOUNDED_CURVE ( )  B_SPLINE_CURVE ( 2, ( #2559, #3870, #14780, #3676, #19370, #5661, #9993, #16093, #2372, #8487, #2175, #19175, #16192 ),
 .UNSPECIFIED., .F., .F. ) 
 B_SPLINE_CURVE_WITH_KNOTS ( ( 3, 2, 2, 2, 2, 2, 3 ),
 ( 0.000000000000000000, 0.05000000000000000278, 0.1000000000000000056, 0.1499999999999999944, 0.2000000000000000111, 0.2500000000000000000, 0.2843253191101273170 ),
 .UNSPECIFIED. ) 
 CURVE ( )  GEOMETRIC_REPRESENTATION_ITEM ( )  RATIONAL_B_SPLINE_CURVE ( ( 1.000000000000000000, 0.9876883405951377704, 1.000000000000000000, 0.9876883405951377704, 1.000000000000000000, 0.9876883405951377704, 1.000000000000000000, 0.9876883405951377704, 1.000000000000000000, 0.9876883405951377704, 1.000000000000000000, 0.9915479672430580482, 0.9947006833465674713 ) ) 
 REPRESENTATION_ITEM ( '' )  );
#17165 = VERTEX_POINT ( 'NONE', #13689 ) ;
#17166 = CARTESIAN_POINT ( 'NONE',  ( -5.209999999999999964, 0.000000000000000000, 0.000000000000000000 ) ) ;
#17167 = CIRCLE ( 'NONE', #8533, 28.06981291497571362 ) ;
#17168 = DIRECTION ( 'NONE',  ( -1.000000000000000000, -0.000000000000000000, -0.000000000000000000 ) ) ;
#17169 = EDGE_CURVE ( 'NONE', #4945, #3153, #2220, .T. ) ;
#17170 = AXIS2_PLACEMENT_3D ( 'NONE', #12586, #7867, #4777 ) ;
#17171 = ORIENTED_EDGE ( 'NONE', *, *, #7731, .F. ) ;
#17172 = DIRECTION ( 'NONE',  ( 0.000000000000000000, 0.000000000000000000, -1.000000000000000000 ) ) ;
#17173 = ORIENTED_EDGE ( 'NONE', *, *, #1128, .F. ) ;
#17174 = AXIS2_PLACEMENT_3D ( 'NONE', #18722, #10833, #6402 ) ;
#17175 = CARTESIAN_POINT ( 'NONE',  ( 2.849999999999954348, -4.936344801571327601, -6.000000000000005329 ) ) ;
#17176 = EDGE_CURVE ( 'NONE', #9264, #6659, #10240, .T. ) ;
#17177 = CARTESIAN_POINT ( 'NONE',  ( 1.039999999999996927, -4.633866840649124796, 27.68468304288256832 ) ) ;
#17178 = FACE_BOUND ( 'NONE', #13950, .T. ) ;
#17179 = VERTEX_POINT ( 'NONE', #19545 ) ;
#17180 = CARTESIAN_POINT ( 'NONE',  ( 9.000000000000000000, 0.000000000000000000, -28.99999999999999645 ) ) ;
#17181 = ORIENTED_EDGE ( 'NONE', *, *, #15518, .T. ) ;
#17182 = ORIENTED_EDGE ( 'NONE', *, *, #7903, .F. ) ;
#17183 = CARTESIAN_POINT ( 'NONE',  ( 2.765633920072235075, -12.59161484032896361, -21.30679549418645280 ) ) ;
#17184 = DIRECTION ( 'NONE',  ( 1.000000000000000000, 0.000000000000000000, 0.000000000000000000 ) ) ;
#17185 = VECTOR ( 'NONE', #699, 1000.000000000000000 ) ;
#17186 = CARTESIAN_POINT ( 'NONE',  ( -1.510506337161861667, 4.648860486681953397, -10.46874999795161720 ) ) ;
#17187 = AXIS2_PLACEMENT_3D ( 'NONE', #2099, #15517, #8101 ) ;
#17188 = VERTEX_POINT ( 'NONE', #16656 ) ;
#17189 = CARTESIAN_POINT ( 'NONE',  ( 10.96874999795161720, 1.773574444220790136, -4.620319390059805187 ) ) ;
#17190 = DIRECTION ( 'NONE',  ( -1.000000000000000000, 0.000000000000000000, 0.000000000000000000 ) ) ;
#17191 = EDGE_LOOP ( 'NONE', ( #16541, #16608 ) ) ;
#17192 = CARTESIAN_POINT ( 'NONE',  ( 0.02436607992776064838, 12.59161484032912171, 21.30679549418635688 ) ) ;
#17193 = CARTESIAN_POINT ( 'NONE',  ( 0.07181524296601550506, -18.89296398180203695, 16.91181672897726784 ) ) ;
#17194 = EDGE_CURVE ( 'NONE', #12265, #11483, #19490, .T. ) ;
#17195 = CYLINDRICAL_SURFACE ( 'NONE', #11572, 22.00000000000000355 ) ;
#17196 = DIRECTION ( 'NONE',  ( 0.000000000000000000, 0.000000000000000000, 1.000000000000000000 ) ) ;
#17197 = CARTESIAN_POINT ( 'NONE',  ( 0.9027913098498173694, -5.700000000000005507, -10.50000000000000711 ) ) ;
#17198 = ORIENTED_EDGE ( 'NONE', *, *, #7561, .F. ) ;
#17199 = VECTOR ( 'NONE', #1658, 999.9999999999998863 ) ;
#17200 = CARTESIAN_POINT ( 'NONE',  ( 12.50000000000000533, 5.142044285764750811, 2.620002426024544029 ) ) ;
#17201 = SURFACE_STYLE_FILL_AREA ( #15698 ) ;
#17202 = FACE_OUTER_BOUND ( 'NONE', #11521, .T. ) ;
#17203 = DIRECTION ( 'NONE',  ( -6.419766481290786633E-33, 1.000000000000000000, 0.000000000000000000 ) ) ;
#17204 = ORIENTED_EDGE ( 'NONE', *, *, #7480, .T. ) ;
#17205 = CARTESIAN_POINT ( 'NONE',  ( -2.000000000000001776, 0.000000000000000000, -7.174999999999999822 ) ) ;
#17206 = DIRECTION ( 'NONE',  ( -1.000000000000000000, 0.000000000000000000, -0.000000000000000000 ) ) ;
#17207 = CARTESIAN_POINT ( 'NONE',  ( 7.968749997951616315, 4.942249507334556924, -0.2590123213420971182 ) ) ;
#17208 = EDGE_CURVE ( 'NONE', #6715, #2313, #13653, .T. ) ;
#17209 = DIRECTION ( 'NONE',  ( 0.9340060080012955179, 0.000000000000000000, -0.3572572980604928339 ) ) ;
#17210 = DIRECTION ( 'NONE',  ( -0.4330127018922234616, -0.7499999999999990008, 0.4999999999999978351 ) ) ;
#17211 = ORIENTED_EDGE ( 'NONE', *, *, #5024, .F. ) ;
#17212 = DIRECTION ( 'NONE',  ( 0.000000000000000000, 0.000000000000000000, -1.000000000000000000 ) ) ;
#17213 = LINE ( 'NONE', #13916, #19738 ) ;
#17214 = ORIENTED_EDGE ( 'NONE', *, *, #3432, .T. ) ;
#17215 = CARTESIAN_POINT ( 'NONE',  ( 7.843749997951614539, -1.510506337161893864, 4.648860486681943627 ) ) ;
#17216 = CARTESIAN_POINT ( 'NONE',  ( 4.476417968967386862, 17.43449690031536292, -32.00000000000000000 ) ) ;
#17217 = AXIS2_PLACEMENT_3D ( 'NONE', #17750, #10154, #16252 ) ;
#17218 = ORIENTED_EDGE ( 'NONE', *, *, #3331, .T. ) ;
#17219 = ADVANCED_FACE ( 'NONE', ( #17962 ), #4162, .T. ) ;
#17220 = PRESENTATION_LAYER_ASSIGNMENT (  '', '', ( #8593 ) ) ;
#17221 = CARTESIAN_POINT ( 'NONE',  ( 2.262072706628479146, -19.66369668717046437, 18.56460150496932116 ) ) ;
#17222 = CARTESIAN_POINT ( 'NONE',  ( 12.65441706489329299, 5.700000000000001954, 0.6173595171471270016 ) ) ;
#17223 = ORIENTED_EDGE ( 'NONE', *, *, #19221, .T. ) ;
#17224 = DIRECTION ( 'NONE',  ( -1.000000000000000000, 0.000000000000000000, 0.000000000000000000 ) ) ;
#17225 =( LENGTH_UNIT ( ) NAMED_UNIT ( * ) SI_UNIT ( .MILLI., .METRE. ) );
#17226 = DIRECTION ( 'NONE',  ( 0.000000000000000000, 1.374038396813314559E-15, -1.000000000000000000 ) ) ;
#17227 = VERTEX_POINT ( 'NONE', #7637 ) ;
#17228 = DIRECTION ( 'NONE',  ( 0.000000000000000000, 0.000000000000000000, 1.000000000000000000 ) ) ;
#17229 = ORIENTED_EDGE ( 'NONE', *, *, #14201, .F. ) ;
#17231 = CARTESIAN_POINT ( 'NONE',  ( 0.5958122406255995651, -5.668774803599162304, -15.31249999590322552 ) ) ;
#17230 = AXIS2_PLACEMENT_3D ( 'NONE', #6542, #17373, #12673 ) ;
#17232 = ORIENTED_EDGE ( 'NONE', *, *, #18777, .F. ) ;
#17233 = FACE_OUTER_BOUND ( 'NONE', #12662, .T. ) ;
#17234 = EDGE_CURVE ( 'NONE', #9467, #8854, #15353, .T. ) ;
#17235 = CARTESIAN_POINT ( 'NONE',  ( 2.999999999999998224, -3.950217066951267064, 3.681818181818180769 ) ) ;
#17236 = CARTESIAN_POINT ( 'NONE',  ( 0.07186811453410689443, 18.89333555428554590, 16.91241718342006450 ) ) ;
#17237 = ORIENTED_EDGE ( 'NONE', *, *, #17570, .F. ) ;
#17238 = DIRECTION ( 'NONE',  ( 0.000000000000000000, 0.000000000000000000, -1.000000000000000000 ) ) ;
#17239 = FACE_OUTER_BOUND ( 'NONE', #1728, .T. ) ;
#17240 = EDGE_LOOP ( 'NONE', ( #2494, #18240, #13864, #13902 ) ) ;
#17241 = CARTESIAN_POINT ( 'NONE',  ( -7.671566133830872047, 15.77352024078954429, 32.00000000000000000 ) ) ;
#17242 = FACE_OUTER_BOUND ( 'NONE', #16873, .T. ) ;
#17243 = EDGE_CURVE ( 'NONE', #13068, #1107, #15688, .T. ) ;
#17244 = CARTESIAN_POINT ( 'NONE',  ( -11.00000000000000355, -4.898587196589412829E-16, 0.000000000000000000 ) ) ;
#17245 = EDGE_CURVE ( 'NONE', #17330, #12027, #19748, .T. ) ;
#17246 = ORIENTED_EDGE ( 'NONE', *, *, #6311, .F. ) ;
#17247 = CARTESIAN_POINT ( 'NONE',  ( 11.50000000000000355, -2.068159791354146293, -5.387740456496247887 ) ) ;
#17248 = CARTESIAN_POINT ( 'NONE',  ( 12.34374999795161543, 3.114526743279308896, -3.846120219227901593 ) ) ;
#17249 = ORIENTED_EDGE ( 'NONE', *, *, #5797, .F. ) ;
#17250 = DIRECTION ( 'NONE',  ( 0.000000000000000000, 0.000000000000000000, -1.000000000000000000 ) ) ;
#17251 = EDGE_CURVE ( 'NONE', #18074, #16953, #5839, .T. ) ;
#17252 = EDGE_LOOP ( 'NONE', ( #15523, #6738, #16520, #10753 ) ) ;
#17253 = SHAPE_DEFINITION_REPRESENTATION ( #16101, #11438 ) ;
#17254 = DIRECTION ( 'NONE',  ( 0.000000000000000000, 0.000000000000000000, 1.000000000000000000 ) ) ;
#17255 = CARTESIAN_POINT ( 'NONE',  ( 14.84374999795161543, -1.988169868018592856, 4.465502636338025688 ) ) ;
#17256 = ORIENTED_EDGE ( 'NONE', *, *, #5523, .F. ) ;
#17257 = ORIENTED_EDGE ( 'NONE', *, *, #18874, .T. ) ;
#17258 = EDGE_CURVE ( 'NONE', #18200, #14637, #10557, .T. ) ;
#17259 = DIRECTION ( 'NONE',  ( 0.000000000000000000, -0.3090169943749486170, 0.9510565162951530871 ) ) ;
#17260 = B_SPLINE_CURVE_WITH_KNOTS ( 'NONE', 3,
 ( #8692, #3996, #14517, #19290, #12908, #13009 ),
 .UNSPECIFIED., .F., .F.,
 ( 4, 2, 4 ),
 ( 4.462636882221863355E-07, 0.001879885203074805429, 0.003759324142461388692 ),
 .UNSPECIFIED. ) ;
#17261 = FACE_OUTER_BOUND ( 'NONE', #7783, .T. ) ;
#17262 = ORIENTED_EDGE ( 'NONE', *, *, #9855, .T. ) ;
#17263 = VECTOR ( 'NONE', #11992, 1000.000000000000000 ) ;
#17264 = AXIS2_PLACEMENT_3D ( 'NONE', #13832, #16938, #3517 ) ;
#17265 = CARTESIAN_POINT ( 'NONE',  ( -4.781284448697179279, 1.016293382781477961, -10.84374999795161543 ) ) ;
#17266 = EDGE_LOOP ( 'NONE', ( #15487, #8882, #3284, #57 ) ) ;
#17267 = DIRECTION ( 'NONE',  ( 1.000000000000000000, 0.000000000000000000, 0.000000000000000000 ) ) ;
#17268 = DIRECTION ( 'NONE',  ( 0.000000000000000000, 0.000000000000000000, -1.000000000000000000 ) ) ;
#17269 =( BOUNDED_SURFACE ( )  B_SPLINE_SURFACE ( 1, 2, ( 
 ( #3247, #8251, #15861, #9362, #1852, #12661, #6630, #11159, #3646, #12758, #10960, #15762, #1755, #4954, #17161, #346, #17255 ),
 ( #2144, #14155, #15465, #9465, #16966, #15659, #18853, #18653, #13959, #3452, #252, #12856, #7943, #1943, #6334, #15560, #654 ) ),
 .UNSPECIFIED., .F., .F., .F. ) 
 B_SPLINE_SURFACE_WITH_KNOTS ( ( 2, 2 ),
 ( 3, 2, 2, 2, 2, 2, 2, 2, 3 ),
 ( 0.000000000000000000, 1.000000000000000000 ),
 ( 0.000000000000000000, 0.05000000000000000278, 0.1000000000000000056, 0.1499999999999999944, 0.2000000000000000111, 0.2500000000000000000, 0.2999999999999999889, 0.3499999999999999778, 0.4000000000000000222 ),
 .UNSPECIFIED. ) 
 GEOMETRIC_REPRESENTATION_ITEM ( )  RATIONAL_B_SPLINE_SURFACE ( (
 ( 1.000000000000000000, 0.9876883405951377704, 1.000000000000000000, 0.9876883405951377704, 1.000000000000000000, 0.9876883405951377704, 1.000000000000000000, 0.9876883405951377704, 1.000000000000000000, 0.9876883405951377704, 1.000000000000000000, 0.9876883405951377704, 1.000000000000000000, 0.9876883405951377704, 1.000000000000000000, 0.9876883405951377704, 1.000000000000000000),
 ( 1.000000000000000000, 0.9876883405951377704, 1.000000000000000000, 0.9876883405951377704, 1.000000000000000000, 0.9876883405951377704, 1.000000000000000000, 0.9876883405951377704, 1.000000000000000000, 0.9876883405951377704, 1.000000000000000000, 0.9876883405951377704, 1.000000000000000000, 0.9876883405951377704, 1.000000000000000000, 0.9876883405951377704, 1.000000000000000000) ) ) 
 REPRESENTATION_ITEM ( '' )  SURFACE ( )  );
#17270 = FACE_BOUND ( 'NONE', #19462, .T. ) ;
#17271 = ORIENTED_EDGE ( 'NONE', *, *, #6193, .T. ) ;
#17272 = AXIS2_PLACEMENT_3D ( 'NONE', #16001, #2978, #16397 ) ;
#17273 = CARTESIAN_POINT ( 'NONE',  ( 0.02436607992775934733, -2.336989772644440855, 24.63872515616082026 ) ) ;
#17274 =( NAMED_UNIT ( * ) SI_UNIT ( $, .STERADIAN. ) SOLID_ANGLE_UNIT ( ) );
#17275 = CONICAL_SURFACE ( 'NONE', #8967, 3.593999999999999861, 0.2132412839022289897 ) ;
#17276 = DIRECTION ( 'NONE',  ( -0.000000000000000000, -0.000000000000000000, -1.000000000000000000 ) ) ;
#17277 = ADVANCED_FACE ( 'NONE', ( #13445, #12157 ), #14860, .F. ) ;
#17278 = ORIENTED_EDGE ( 'NONE', *, *, #19688, .T. ) ;
#17279 = ORIENTED_EDGE ( 'NONE', *, *, #9049, .F. ) ;
#17280 = ADVANCED_FACE ( 'NONE', ( #1155 ), #11208, .T. ) ;
#17281 = DIRECTION ( 'NONE',  ( 0.000000000000000000, 0.000000000000000000, 1.000000000000000000 ) ) ;
#17282 = DIRECTION ( 'NONE',  ( 0.000000000000000000, 0.000000000000000000, 1.000000000000000000 ) ) ;
#17283 = ORIENTED_EDGE ( 'NONE', *, *, #16051, .F. ) ;
#17284 = ADVANCED_FACE ( 'NONE', ( #12058 ), #15048, .T. ) ;
#17285 = DIRECTION ( 'NONE',  ( -0.4999999999999977240, -0.7499999999999961142, -0.4330127018922284576 ) ) ;
#17286 = LINE ( 'NONE', #3575, #7207 ) ;
#17287 = AXIS2_PLACEMENT_3D ( 'NONE', #14419, #4003, #17710 ) ;
#17288 = VERTEX_POINT ( 'NONE', #2739 ) ;
#17289 = CARTESIAN_POINT ( 'NONE',  ( 17.11901729331276556, 5.562305898749055011, 35.00000000000000000 ) ) ;
#17290 = DIRECTION ( 'NONE',  ( 0.000000000000000000, 0.000000000000000000, 1.000000000000000000 ) ) ;
#17291 = EDGE_CURVE ( 'NONE', #4727, #14720, #10364, .T. ) ;
#17292 = ADVANCED_FACE ( 'NONE', ( #16464 ), #1248, .T. ) ;
#17293 = CARTESIAN_POINT ( 'NONE',  ( -8.000000000000000000, 0.000000000000000000, -29.00000000000000000 ) ) ;
#17294 = FACE_OUTER_BOUND ( 'NONE', #177, .T. ) ;
#17295 = CARTESIAN_POINT ( 'NONE',  ( 5.700000000000001066, -3.980288726281172656E-14, -6.000000000000005329 ) ) ;
#17296 = DIRECTION ( 'NONE',  ( -1.000000000000000000, -6.419766481290786633E-33, 0.000000000000000000 ) ) ;
#17297 = DIRECTION ( 'NONE',  ( 0.000000000000000000, -1.000000000000000000, 0.000000000000000000 ) ) ;
#17298 = CARTESIAN_POINT ( 'NONE',  ( 2.789999999999999147, 18.28042085475278355, 15.74360496233388140 ) ) ;
#17299 = VERTEX_POINT ( 'NONE', #8953 ) ;
#17300 = CARTESIAN_POINT ( 'NONE',  ( 0.02436607992776368414, -9.836394144775550075, -22.71065055754462492 ) ) ;
#17301 = AXIS2_PLACEMENT_3D ( 'NONE', #18254, #143, #2932 ) ;
#17302 = AXIS2_PLACEMENT_3D ( 'NONE', #13844, #15448, #7728 ) ;
#17303 = DIRECTION ( 'NONE',  ( 0.000000000000000000, 1.224646799147333486E-16, 1.000000000000000000 ) ) ;
#17304 = TOROIDAL_SURFACE ( 'NONE', #17954, 24.12539914357697413, 8.000000000000000000 ) ;
#17305 = CARTESIAN_POINT ( 'NONE',  ( -2.000000000000001776, 0.000000000000000000, 0.000000000000000000 ) ) ;
#17306 = DIRECTION ( 'NONE',  ( 1.000000000000000000, 0.000000000000000000, 0.000000000000000000 ) ) ;
#17307 = ORIENTED_EDGE ( 'NONE', *, *, #10527, .T. ) ;
#17308 = FACE_OUTER_BOUND ( 'NONE', #7309, .T. ) ;
#17309 = FACE_OUTER_BOUND ( 'NONE', #3386, .T. ) ;
#17310 = ORIENTED_EDGE ( 'NONE', *, *, #9951, .T. ) ;
#17311 = CARTESIAN_POINT ( 'NONE',  ( 11.31249999590322375, -5.421022142882388373, 1.761396867937162769 ) ) ;
#17312 = EDGE_CURVE ( 'NONE', #19582, #6940, #8007, .T. ) ;
#17313 = CARTESIAN_POINT ( 'NONE',  ( 1.039999999999996705, 27.76164181293051669, -4.147968289691385202 ) ) ;
#17314 = EDGE_LOOP ( 'NONE', ( #13269, #13335 ) ) ;
#17315 = ADVANCED_FACE ( 'NONE', ( #19654 ), #18163, .F. ) ;
#17316 = VECTOR ( 'NONE', #11926, 1000.000000000000000 ) ;
#17317 = CIRCLE ( 'NONE', #2925, 1.000000000000000888 ) ;
#17318 = ADVANCED_FACE ( 'NONE', ( #1450 ), #12817, .T. ) ;
#17319 = CARTESIAN_POINT ( 'NONE',  ( 0.000000000000000000, 4.000000000000000000, 0.000000000000000000 ) ) ;
#17320 = CARTESIAN_POINT ( 'NONE',  ( 10.31249999590322552, 4.611396867937201272, -3.350375938067097437 ) ) ;
#17321 = VERTEX_POINT ( 'NONE', #19108 ) ;
#17322 = LINE ( 'NONE', #3712, #8831 ) ;
#17323 = CARTESIAN_POINT ( 'NONE',  ( -5.575441324182679459, 1.185096637661293251, -11.31249999590322375 ) ) ;
#17324 = DIRECTION ( 'NONE',  ( 1.000000000000000000, 0.000000000000000000, 0.000000000000000000 ) ) ;
#17325 = AXIS2_PLACEMENT_3D ( 'NONE', #15290, #2668, #7665 ) ;
#17326 = VERTEX_POINT ( 'NONE', #11511 ) ;
#17327 = LINE ( 'NONE', #8519, #14061 ) ;
#17328 = ORIENTED_EDGE ( 'NONE', *, *, #11910, .F. ) ;
#17329 = CARTESIAN_POINT ( 'NONE',  ( -12.32184790671639085, 13.12143529358541549, 35.00000000000000000 ) ) ;
#17330 = VERTEX_POINT ( 'NONE', #5493 ) ;
#17331 = ADVANCED_FACE ( 'NONE', ( #9828 ), #16308, .T. ) ;
#17332 = CARTESIAN_POINT ( 'NONE',  ( 0.000000000000000000, 0.000000000000000000, 0.000000000000000000 ) ) ;
#17333 = CARTESIAN_POINT ( 'NONE',  ( 0.7592463965288815952, 12.98165646470117274, -24.32906614999601302 ) ) ;
#17334 = CARTESIAN_POINT ( 'NONE',  ( 1.749999999999998002, 19.67366047555558950, -20.02152543075324687 ) ) ;
#17335 = CIRCLE ( 'NONE', #5180, 0.03079999999999836341 ) ;
#17336 = DIRECTION ( 'NONE',  ( 0.000000000000000000, -0.9510565162951544194, 0.3090169943749446757 ) ) ;
#17337 = VERTEX_POINT ( 'NONE', #16124 ) ;
#17338 = AXIS2_PLACEMENT_3D ( 'NONE', #7670, #15298, #4879 ) ;
#17339 = FACE_BOUND ( 'NONE', #13233, .T. ) ;
#17340 = FACE_OUTER_BOUND ( 'NONE', #17132, .T. ) ;
#17341 = VERTEX_POINT ( 'NONE', #2397 ) ;
#17342 = AXIS2_PLACEMENT_3D ( 'NONE', #12163, #10272, #10565 ) ;
#17343 = DIRECTION ( 'NONE',  ( -0.000000000000000000, -0.000000000000000000, 1.000000000000000000 ) ) ;
#17344 = ADVANCED_FACE ( 'NONE', ( #7076 ), #13764, .T. ) ;
#17345 = CARTESIAN_POINT ( 'NONE',  ( 2.500000000000002220, 0.000000000000000000, 0.000000000000000000 ) ) ;
#17346 = CARTESIAN_POINT ( 'NONE',  ( -4.233219804643904460, -2.444050593749961031, -11.46874999795161543 ) ) ;
#17347 = ADVANCED_BREP_SHAPE_REPRESENTATION ( '', ( #16178, #16724 ), #3632 ) ;
#17348 = ORIENTED_EDGE ( 'NONE', *, *, #7969, .F. ) ;
#17349 = AXIS2_PLACEMENT_3D ( 'NONE', #16787, #9178, #15283 ) ;
#17350 = DIRECTION ( 'NONE',  ( 1.000000000000000000, 6.419766481290786633E-33, -0.000000000000000000 ) ) ;
#17351 = CARTESIAN_POINT ( 'NONE',  ( 7.343749997951615427, -3.846120219227901149, -3.114526743279308896 ) ) ;
#17352 = ORIENTED_EDGE ( 'NONE', *, *, #16877, .T. ) ;
#17353 = DIRECTION ( 'NONE',  ( 1.000000000000000000, 0.000000000000000000, 0.000000000000000000 ) ) ;
#17354 = ORIENTED_EDGE ( 'NONE', *, *, #9460, .F. ) ;
#17355 = CIRCLE ( 'NONE', #97, 3.323500000000020993 ) ;
#17356 = CONTEXT_DEPENDENT_SHAPE_REPRESENTATION ( #16903, #19125 ) ;
#17357 = CARTESIAN_POINT ( 'NONE',  ( 11.34374999795161543, -1.773574444220757274, 4.620319390059819398 ) ) ;
#17358 = DIRECTION ( 'NONE',  ( -1.000000000000000000, 0.000000000000000000, 0.000000000000000000 ) ) ;
#17359 =( GEOMETRIC_REPRESENTATION_CONTEXT ( 3 ) GLOBAL_UNCERTAINTY_ASSIGNED_CONTEXT ( ( #14606 ) ) GLOBAL_UNIT_ASSIGNED_CONTEXT ( ( #9716, #4903, #9414 ) ) REPRESENTATION_CONTEXT ( 'NONE', 'WORKASPACE' ) );
#17360 = VERTEX_POINT ( 'NONE', #11605 ) ;
#17361 = ORIENTED_EDGE ( 'NONE', *, *, #18232, .F. ) ;
#17362 = CARTESIAN_POINT ( 'NONE',  ( 7.937499999999996447, -4.582717761692668645, -0.7089489049740167470 ) ) ;
#17363 = CARTESIAN_POINT ( 'NONE',  ( -6.626241948324210540, -16.73597674598852336, 32.00000000000000000 ) ) ;
#17364 = DIRECTION ( 'NONE',  ( -1.000000000000000000, 0.000000000000000000, -0.000000000000000000 ) ) ;
#17365 = ORIENTED_EDGE ( 'NONE', *, *, #7750, .T. ) ;
#17366 = EDGE_CURVE ( 'NONE', #5957, #18333, #19200, .T. ) ;
#17367 = APPLICATION_CONTEXT ( 'automotive_design' ) ;
#17368 = PRODUCT ( 'Outer Wheel Hub Shell', 'Outer Wheel Hub Shell', '', ( #1651 ) ) ;
#17369 = VERTEX_POINT ( 'NONE', #15918 ) ;
#17370 = EDGE_CURVE ( 'NONE', #11363, #15591, #18001, .T. ) ;
#17371 = EDGE_CURVE ( 'NONE', #9559, #15354, #10212, .T. ) ;
#17372 = B_SPLINE_CURVE_WITH_KNOTS ( 'NONE', 3,
 ( #1187, #13099, #11891, #1287 ),
 .UNSPECIFIED., .F., .F.,
 ( 4, 4 ),
 ( 3.059063720746937335E-07, 0.0006888942284914199117 ),
 .UNSPECIFIED. ) ;
#17373 = DIRECTION ( 'NONE',  ( 0.000000000000000000, 0.000000000000000000, 1.000000000000000000 ) ) ;
#17374 = FACE_OUTER_BOUND ( 'NONE', #6344, .T. ) ;
#17375 = CARTESIAN_POINT ( 'NONE',  ( 1.749999999999998002, -12.96210679857804671, 24.89775460606827551 ) ) ;
#17376 = EDGE_LOOP ( 'NONE', ( #2165, #14932 ) ) ;
#17377 = CARTESIAN_POINT ( 'NONE',  ( 0.7592463965288811512, -24.32906614999605921, -12.98165646470108925 ) ) ;
#17378 = CARTESIAN_POINT ( 'NONE',  ( 1.280903732194454303, 4.780397808154257078, -8.968749997951611874 ) ) ;
#17379 = ORIENTED_EDGE ( 'NONE', *, *, #1949, .F. ) ;
#17380 = EDGE_LOOP ( 'NONE', ( #4980, #17310, #3520, #11100 ) ) ;
#17381 = CARTESIAN_POINT ( 'NONE',  ( 18.68117051311639543, -3.372863662543048591, -35.00000000000000000 ) ) ;
#17382 = CLOSED_SHELL ( 'NONE', ( #12582, #9349, #15860, #1662, #10581, #9725, #13968, #11509, #12916 ) ) ;
#17383 = CIRCLE ( 'NONE', #3972, 0.03079999999999923077 ) ;
#17384 = CARTESIAN_POINT ( 'NONE',  ( -3.000000000000002665, 0.000000000000000000, 0.000000000000000000 ) ) ;
#17385 = DIRECTION ( 'NONE',  ( 0.000000000000000000, 0.000000000000000000, -1.000000000000000000 ) ) ;
#17386 = ORIENTED_EDGE ( 'NONE', *, *, #18223, .T. ) ;
#17387 = DIRECTION ( 'NONE',  ( -0.000000000000000000, -0.000000000000000000, 1.000000000000000000 ) ) ;
#17388 = DIRECTION ( 'NONE',  ( -0.4999999999999979461, 0.7500000000000021094, -0.4330127018922180770 ) ) ;
#17389 =( GEOMETRIC_REPRESENTATION_CONTEXT ( 3 ) GLOBAL_UNCERTAINTY_ASSIGNED_CONTEXT ( ( #4384 ) ) GLOBAL_UNIT_ASSIGNED_CONTEXT ( ( #6648, #11276, #17274 ) ) REPRESENTATION_CONTEXT ( 'NONE', 'WORKASPACE' ) );
#17390 = AXIS2_PLACEMENT_3D ( 'NONE', #8345, #9764, #16052 ) ;
#17391 = ORIENTED_EDGE ( 'NONE', *, *, #2228, .T. ) ;
#17392 = LINE ( 'NONE', #11389, #6855 ) ;
#17393 = ADVANCED_FACE ( 'NONE', ( #2201 ), #13210, .T. ) ;
#17394 = EDGE_CURVE ( 'NONE', #7691, #15645, #6395, .T. ) ;
#17395 = CARTESIAN_POINT ( 'NONE',  ( -10.00000000000000000, 0.000000000000000000, 0.000000000000000000 ) ) ;
#17396 = CIRCLE ( 'NONE', #6519, 0.9999999999999974465 ) ;
#17397 = DIRECTION ( 'NONE',  ( 1.000000000000000000, 0.000000000000000000, 0.000000000000000000 ) ) ;
#17398 = CARTESIAN_POINT ( 'NONE',  ( 2.783068930044319433, 18.43696893154781691, -16.17493693894858353 ) ) ;
#17399 = DIRECTION ( 'NONE',  ( 1.000000000000000000, 0.000000000000000000, 0.000000000000000000 ) ) ;
#17400 = DIRECTION ( 'NONE',  ( 0.000000000000000000, 5.496153587253259026E-15, -1.000000000000000000 ) ) ;
#17401 = DIRECTION ( 'NONE',  ( 1.000000000000000000, 0.000000000000000000, 0.000000000000000000 ) ) ;
#17402 = CARTESIAN_POINT ( 'NONE',  ( 1.039999999999997593, 0.000000000000000000, 0.000000000000000000 ) ) ;
#17403 = ORIENTED_EDGE ( 'NONE', *, *, #19468, .T. ) ;
#17404 = EDGE_CURVE ( 'NONE', #13068, #12768, #2562, .T. ) ;
#17405 = CARTESIAN_POINT ( 'NONE',  ( 5.294050593750000644, -3.696815770993907903E-14, -7.078124996927420476 ) ) ;
#17406 = SURFACE_STYLE_USAGE ( .BOTH. , #12705 ) ;
#17407 = PRODUCT_DEFINITION_CONTEXT ( 'detailed design', #17367, 'design' ) ;
#17408 = CARTESIAN_POINT ( 'NONE',  ( 4.936344801571289409, -2.850000000000023626, -12.31249999590322552 ) ) ;
#17409 = CARTESIAN_POINT ( 'NONE',  ( 12.00000000000000533, -4.235925505221167064, 3.814044456245474279 ) ) ;
#17410 = DIRECTION ( 'NONE',  ( 0.000000000000000000, 0.000000000000000000, 1.000000000000000000 ) ) ;
#17411 = VERTEX_POINT ( 'NONE', #6890 ) ;
#17412 = DIRECTION ( 'NONE',  ( -1.000000000000000000, 0.000000000000000000, -0.000000000000000000 ) ) ;
#17413 = CARTESIAN_POINT ( 'NONE',  ( 2.444050593749960587, -4.233219804643904460, -6.843749997951615427 ) ) ;
#17415 = EDGE_CURVE ( 'NONE', #4109, #12630, #5307, .T. ) ;
#17414 = EDGE_CURVE ( 'NONE', #3340, #19072, #1521, .T. ) ;
#17416 = EDGE_LOOP ( 'NONE', ( #15812, #2005, #6432, #1624 ) ) ;
#17417 = AXIS2_PLACEMENT_3D ( 'NONE', #7887, #1892, #17297 ) ;
#17418 = CARTESIAN_POINT ( 'NONE',  ( 10.84374999795161543, -4.648860486681964055, 1.510506337161829027 ) ) ;
#17419 = CYLINDRICAL_SURFACE ( 'NONE', #8835, 1.000000000000004441 ) ;
#17420 = ORIENTED_EDGE ( 'NONE', *, *, #1594, .T. ) ;
#17421 = FACE_OUTER_BOUND ( 'NONE', #15271, .T. ) ;
#17422 = CARTESIAN_POINT ( 'NONE',  ( 0.02436607992776455150, 5.391175441198956086, -24.15498966839956907 ) ) ;
#17423 = VECTOR ( 'NONE', #8650, 1000.000000000000000 ) ;
#17424 = LINE ( 'NONE', #217, #1970 ) ;
#17425 = CARTESIAN_POINT ( 'NONE',  ( 2.790000000000077307, 22.38018801136476554, 9.515416771311276278 ) ) ;
#17426 = VERTEX_POINT ( 'NONE', #12915 ) ;
#17427 = CARTESIAN_POINT ( 'NONE',  ( 6.234374998975811266, -4.584782303107616031, 2.647025296874957689 ) ) ;
#17428 = CARTESIAN_POINT ( 'NONE',  ( 0.000000000000000000, 0.000000000000000000, 0.000000000000000000 ) ) ;
#17429 = PLANE ( 'NONE',  #15484 ) ;
#17430 = ORIENTED_EDGE ( 'NONE', *, *, #285, .T. ) ;
#17431 = CARTESIAN_POINT ( 'NONE',  ( 11.96874999795161365, -4.888101187499994893, -0.7741991708319226895 ) ) ;
#17432 = ORIENTED_EDGE ( 'NONE', *, *, #15895, .T. ) ;
#17433 = DIRECTION ( 'NONE',  ( 0.000000000000000000, 0.000000000000000000, 1.000000000000000000 ) ) ;
#17434 = VERTEX_POINT ( 'NONE', #11416 ) ;
#17435 = DIRECTION ( 'NONE',  ( 1.000000000000000000, 0.000000000000000000, 0.000000000000000000 ) ) ;
#17436 = DIRECTION ( 'NONE',  ( 1.000000000000000000, 0.000000000000000000, 0.000000000000000000 ) ) ;
#17437 = DIRECTION ( 'NONE',  ( 0.000000000000000000, 0.000000000000000000, 1.000000000000000000 ) ) ;
#17438 = CIRCLE ( 'NONE', #14873, 0.03079999999999923077 ) ;
#17439 = CARTESIAN_POINT ( 'NONE',  ( 1.988169868018562880, -4.465502636338038123, -13.84374999795161543 ) ) ;
#17440 = CIRCLE ( 'NONE', #182, 6.799999999999998046 ) ;
#17441 = ORIENTED_EDGE ( 'NONE', *, *, #17857, .T. ) ;
#17442 = FACE_OUTER_BOUND ( 'NONE', #7073, .T. ) ;
#17443 = B_SPLINE_CURVE_WITH_KNOTS ( 'NONE', 3,
 ( #5116, #17333, #630, #3623, #17137, #8227 ),
 .UNSPECIFIED., .F., .F.,
 ( 4, 2, 4 ),
 ( 4.462636695653741059E-07, 0.001879885036799761131, 0.003759323809929956614 ),
 .UNSPECIFIED. ) ;
#17444 = LINE ( 'NONE', #3529, #5289 ) ;
#17445 = ORIENTED_EDGE ( 'NONE', *, *, #11969, .F. ) ;
#17446 = CARTESIAN_POINT ( 'NONE',  ( 6.843749997951615427, -4.233219804643904460, 2.444050593749960587 ) ) ;
#17447 = DIRECTION ( 'NONE',  ( 0.000000000000000000, 0.000000000000000000, 1.000000000000000000 ) ) ;
#17448 = CYLINDRICAL_SURFACE ( 'NONE', #3294, 4.200000000000000178 ) ;
#17449 = EDGE_LOOP ( 'NONE', ( #18157, #6699, #14432, #6675 ) ) ;
#17450 = AXIS2_PLACEMENT_3D ( 'NONE', #7226, #7327, #10461 ) ;
#17451 = FACE_OUTER_BOUND ( 'NONE', #18848, .T. ) ;
#17452 = CYLINDRICAL_SURFACE ( 'NONE', #15223, 1.000000000000002665 ) ;
#17453 = DIRECTION ( 'NONE',  ( 1.000000000000000000, 1.224646799147353207E-16, -0.000000000000000000 ) ) ;
#17454 = AXIS2_PLACEMENT_3D ( 'NONE', #17216, #9728, #3703 ) ;
#17455 = VERTEX_POINT ( 'NONE', #3805 ) ;
#17456 = FACE_OUTER_BOUND ( 'NONE', #2323, .T. ) ;
#17457 = EDGE_LOOP ( 'NONE', ( #10466, #7617, #1783, #18005 ) ) ;
#17458 = ITEM_DEFINED_TRANSFORMATION ( 'NONE', 'NONE', #4438,  #16724 ) ;
#17459 = CYLINDRICAL_SURFACE ( 'NONE', #8724, 3.968750000000000000 ) ;
#17460 = CARTESIAN_POINT ( 'NONE',  ( 2.718184767880468922, -23.19431517146925970, -10.24584646439563507 ) ) ;
#17461 = ORIENTED_EDGE ( 'NONE', *, *, #19221, .F. ) ;
#17462 = EDGE_LOOP ( 'NONE', ( #17703, #403, #13742, #6651 ) ) ;
#17463 = CARTESIAN_POINT ( 'NONE',  ( 0.000000000000000000, 0.000000000000000000, 0.000000000000000000 ) ) ;
#17464 = CARTESIAN_POINT ( 'NONE',  ( 13.00000000000000178, -1.070668164103420805, -5.063333171156729762 ) ) ;
#17465 = ADVANCED_FACE ( 'NONE', ( #16014, #2301 ), #16215, .T. ) ;
#17466 = VERTEX_POINT ( 'NONE', #2490 ) ;
#17467 = AXIS2_PLACEMENT_3D ( 'NONE', #341, #6420, #12557 ) ;
#17468 = CIRCLE ( 'NONE', #1807, 24.12539914357697768 ) ;
#17469 = ORIENTED_EDGE ( 'NONE', *, *, #5198, .T. ) ;
#17470 = FACE_OUTER_BOUND ( 'NONE', #1365, .T. ) ;
#17471 = CARTESIAN_POINT ( 'NONE',  ( 0.000000000000000000, 0.000000000000000000, -33.00000000000000000 ) ) ;
#17472 = EDGE_CURVE ( 'NONE', #5267, #1462, #6913, .T. ) ;
#17473 = CARTESIAN_POINT ( 'NONE',  ( -4.465502636338051445, -1.988169868018530462, -8.843749997951615427 ) ) ;
#17474 = VECTOR ( 'NONE', #11396, 1000.000000000000000 ) ;
#17475 = EDGE_LOOP ( 'NONE', ( #14322, #904, #5953, #3347 ) ) ;
#17476 = CARTESIAN_POINT ( 'NONE',  ( 0.000000000000000000, 0.000000000000000000, 0.000000000000000000 ) ) ;
#17477 = CARTESIAN_POINT ( 'NONE',  ( -0.2590123213420971182, 4.942249507334556924, -7.968749997951616315 ) ) ;
#17478 = AXIS2_PLACEMENT_3D ( 'NONE', #18927, #8324, #17436 ) ;
#17479 = ORIENTED_EDGE ( 'NONE', *, *, #15178, .F. ) ;
#17480 = ORIENTED_EDGE ( 'NONE', *, *, #8714, .T. ) ;
#17481 = CARTESIAN_POINT ( 'NONE',  ( -4.861323657744413218, -0.5109457054261099529, -9.468749997951615427 ) ) ;
#17482 = EDGE_CURVE ( 'NONE', #9454, #4538, #9001, .T. ) ;
#17483 = DIRECTION ( 'NONE',  ( 1.000000000000000000, 0.000000000000000000, 0.000000000000000000 ) ) ;
#17484 = CARTESIAN_POINT ( 'NONE',  ( 2.255998204157473097, -17.85806462366060288, -32.00000000000000000 ) ) ;
#17485 = VERTEX_POINT ( 'NONE', #4489 ) ;
#17486 = CARTESIAN_POINT ( 'NONE',  ( 11.84374999795161365, 2.444050593750049405, -4.233219804643852946 ) ) ;
#17487 = AXIS2_PLACEMENT_3D ( 'NONE', #15482, #18971, #8638 ) ;
#17488 = EDGE_LOOP ( 'NONE', ( #7385, #18822 ) ) ;
#17489 = CARTESIAN_POINT ( 'NONE',  ( 6.656249997951614539, -4.233219804643904460, 2.444050593749960587 ) ) ;
#17490 = AXIS2_PLACEMENT_3D ( 'NONE', #17562, #11554, #16168 ) ;
#17491 = FACE_OUTER_BOUND ( 'NONE', #15078, .T. ) ;
#17492 = PLANE ( 'NONE',  #8700 ) ;
#17493 = CARTESIAN_POINT ( 'NONE',  ( 0.0003207540509378258692, 20.70663861606293921, -12.51925356660738053 ) ) ;
#17494 = EDGE_CURVE ( 'NONE', #4466, #15252, #10552, .T. ) ;
#17495 = CARTESIAN_POINT ( 'NONE',  ( 3.350375938067065462, -4.611396867937225252, -9.000000000000005329 ) ) ;
#17496 = CARTESIAN_POINT ( 'NONE',  ( -13.86923836996420967, -11.47363181547641275, -32.00000000000000000 ) ) ;
#17497 = CARTESIAN_POINT ( 'NONE',  ( 7.937500000000000000, -3.073999505363504081, -0.3133235625263147694 ) ) ;
#17498 = DIRECTION ( 'NONE',  ( 0.000000000000000000, -0.5877852522924743583, 0.8090169943749465631 ) ) ;
#17499 = ORIENTED_EDGE ( 'NONE', *, *, #8757, .F. ) ;
#17500 = DIRECTION ( 'NONE',  ( -0.000000000000000000, -0.000000000000000000, -1.000000000000000000 ) ) ;
#17501 = EDGE_CURVE ( 'NONE', #1763, #6045, #10702, .T. ) ;
#17502 = AXIS2_PLACEMENT_3D ( 'NONE', #5696, #4405, #5898 ) ;
#17503 = CARTESIAN_POINT ( 'NONE',  ( -34.92499999999994742, 0.000000000000000000, 0.000000000000000000 ) ) ;
#17504 = LINE ( 'NONE', #3793, #13121 ) ;
#17505 = AXIS2_PLACEMENT_3D ( 'NONE', #2414, #10132, #3921 ) ;
#17506 = LINE ( 'NONE', #10013, #9246 ) ;
#17507 = ADVANCED_FACE ( 'NONE', ( #16812 ), #9293, .T. ) ;
#17508 = FACE_OUTER_BOUND ( 'NONE', #3021, .T. ) ;
#17509 = VERTEX_POINT ( 'NONE', #5888 ) ;
#17510 = CARTESIAN_POINT ( 'NONE',  ( 14.31249999590322552, -4.611396867937178179, -3.350375938067128967 ) ) ;
#17511 = CARTESIAN_POINT ( 'NONE',  ( 0.7592463941534238758, 27.31305418910209681, -3.797885586973310801 ) ) ;
#17512 = ORIENTED_EDGE ( 'NONE', *, *, #8103, .F. ) ;
#17513 = CARTESIAN_POINT ( 'NONE',  ( 4.098876516494237640E-16, -15.96500990068138570, 18.34424029220106078 ) ) ;
#17514 = EDGE_CURVE ( 'NONE', #7908, #7464, #16970, .T. ) ;
#17515 = CARTESIAN_POINT ( 'NONE',  ( 0.000000000000000000, 0.000000000000000000, 0.000000000000000000 ) ) ;
#17516 = CIRCLE ( 'NONE', #7586, 4.000000000000000000 ) ;
#17517 = CIRCLE ( 'NONE', #14005, 4.000000000000000000 ) ;
#17518 = DIRECTION ( 'NONE',  ( 0.000000000000000000, 0.000000000000000000, -1.000000000000000000 ) ) ;
#17519 = DIRECTION ( 'NONE',  ( -0.9773501006361902110, 0.000000000000000000, 0.2116288751244233268 ) ) ;
#17520 = VERTEX_POINT ( 'NONE', #3088 ) ;
#17521 = CARTESIAN_POINT ( 'NONE',  ( 4.611396867937200383, 3.350375938067097881, -14.00000000000000533 ) ) ;
#17522 = SURFACE_STYLE_USAGE ( .BOTH. , #11423 ) ;
#17523 = EDGE_CURVE ( 'NONE', #4538, #871, #1198, .T. ) ;
#17524 = CARTESIAN_POINT ( 'NONE',  ( 1.749999999999998002, -20.02152543075331081, -19.67366047555553266 ) ) ;
#17525 = ADVANCED_FACE ( 'NONE', ( #19600 ), #2989, .F. ) ;
#17526 = EDGE_LOOP ( 'NONE', ( #9290, #6306, #1304, #16937, #10666, #8299 ) ) ;
#17527 = CARTESIAN_POINT ( 'NONE',  ( 13.46874999795161543, -3.954556930911842016, -2.873153789725852558 ) ) ;
#17528 = VERTEX_POINT ( 'NONE', #1401 ) ;
#17529 = CARTESIAN_POINT ( 'NONE',  ( -2.850000000000058265, -4.936344801571268093, -6.656249997951614539 ) ) ;
#17530 = EDGE_LOOP ( 'NONE', ( #6134, #15185, #10677, #18077, #6198, #280 ) ) ;
#17531 = CARTESIAN_POINT ( 'NONE',  ( 16.68117051311640253, -3.372863662543048591, 35.00000000000000000 ) ) ;
#17532 = CARTESIAN_POINT ( 'NONE',  ( -6.929096493834647319, 2.870125742738179664, 0.000000000000000000 ) ) ;
#17533 = PRODUCT ( 'brake arm', 'brake arm', '', ( #9661 ) ) ;
#17534 = CARTESIAN_POINT ( 'NONE',  ( 12.00000000000000000, 0.000000000000000000, 0.000000000000000000 ) ) ;
#17535 = CIRCLE ( 'NONE', #3784, 1.000000000000002665 ) ;
#17536 = CARTESIAN_POINT ( 'NONE',  ( -22.50000000000000711, 21.04737509655562988, -2.577560054245056178E-15 ) ) ;
#17537 = VERTEX_POINT ( 'NONE', #8801 ) ;
#17538 = CARTESIAN_POINT ( 'NONE',  ( 1.016293382781377819, -4.781284448697200595, -7.843749997951614539 ) ) ;
#17539 = CARTESIAN_POINT ( 'NONE',  ( 10.98069898359950258, -0.5990941410143687529, 5.700000000000001954 ) ) ;
#17540 = ORIENTED_EDGE ( 'NONE', *, *, #11293, .F. ) ;
#17541 = EDGE_CURVE ( 'NONE', #16734, #10744, #8335, .T. ) ;
#17542 = EDGE_CURVE ( 'NONE', #18804, #17931, #5981, .T. ) ;
#17543 = DIRECTION ( 'NONE',  ( -1.000000000000000000, 0.000000000000000000, 0.000000000000000000 ) ) ;
#17544 = DIRECTION ( 'NONE',  ( 1.000000000000000000, 0.000000000000000000, 0.000000000000000000 ) ) ;
#17545 = CARTESIAN_POINT ( 'NONE',  ( 3.499494075959791672, -3.499494075959840966, -9.343749997951615427 ) ) ;
#17546 = ADVANCED_FACE ( 'NONE', ( #18207 ), #15525, .F. ) ;
#17547 = AXIS2_PLACEMENT_3D ( 'NONE', #12664, #15766, #2347 ) ;
#17548 = VERTEX_POINT ( 'NONE', #13899 ) ;
#17549 = DIRECTION ( 'NONE',  ( 0.000000000000000000, 1.000000000000000000, 0.000000000000000000 ) ) ;
#17550 = CARTESIAN_POINT ( 'NONE',  ( 3.954556930911842016, -2.873153789725853002, -8.468749997951615427 ) ) ;
#17551 = CARTESIAN_POINT ( 'NONE',  ( -2.000000000000000000, 4.999999999999998224, 41.99999999999999289 ) ) ;
#17552 = ORIENTED_EDGE ( 'NONE', *, *, #883, .T. ) ;
#17553 = CARTESIAN_POINT ( 'NONE',  ( 0.7589665203264078785, 19.12621924769895898, -19.86422722021291776 ) ) ;
#17554 = VERTEX_POINT ( 'NONE', #14087 ) ;
#17555 = DIRECTION ( 'NONE',  ( -1.000000000000000000, -6.419766481290786633E-33, 0.000000000000000000 ) ) ;
#17556 = MECHANICAL_DESIGN_GEOMETRIC_PRESENTATION_REPRESENTATION (  '', ( #11469 ), #5390 ) ;
#17557 = DIRECTION ( 'NONE',  ( 1.000000000000000000, 0.000000000000000000, 0.000000000000000000 ) ) ;
#17558 = DIRECTION ( 'NONE',  ( 0.000000000000000000, 0.000000000000000000, 1.000000000000000000 ) ) ;
#17559 = ORIENTED_EDGE ( 'NONE', *, *, #4889, .F. ) ;
#17560 = CARTESIAN_POINT ( 'NONE',  ( 2.246813503491803310, -4.409619785863921670, -10.34374999795161543 ) ) ;
#17561 = CARTESIAN_POINT ( 'NONE',  ( 11.81249999590322552, -5.700000000000006395, 0.9027913098498173694 ) ) ;
#17562 = CARTESIAN_POINT ( 'NONE',  ( 0.000000000000000000, 7.909232158574813099, 24.34211360614303388 ) ) ;
#17563 = EDGE_LOOP ( 'NONE', ( #17694, #3677 ) ) ;
#17564 = CIRCLE ( 'NONE', #2518, 0.03079999999999923077 ) ;
#17565 = EDGE_CURVE ( 'NONE', #1584, #3868, #9596, .T. ) ;
#17566 = CIRCLE ( 'NONE', #15328, 8.000000000000000000 ) ;
#17567 = ORIENTED_EDGE ( 'NONE', *, *, #1008, .F. ) ;
#17568 = SHAPE_REPRESENTATION ( 'angular contact ball bearing_68_iso_ISO 15 ABB - 188 - 12,SI,NC,12_68', ( #16724 ), #16113 ) ;
#17569 = DIRECTION ( 'NONE',  ( -0.000000000000000000, -0.000000000000000000, 1.000000000000000000 ) ) ;
#17570 = EDGE_CURVE ( 'NONE', #12690, #13049, #2262, .T. ) ;
#17571 = CARTESIAN_POINT ( 'NONE',  ( 14.19790265903627180, 9.644882309621939598, 35.00000000000000000 ) ) ;
#17572 = ORIENTED_EDGE ( 'NONE', *, *, #16098, .T. ) ;
#17573 = CARTESIAN_POINT ( 'NONE',  ( -3.270778111535288080, 3.632567103900569361, -12.46874999795161543 ) ) ;
#17574 = FILL_AREA_STYLE_COLOUR ( '', #14669 ) ;
#17575 = ORIENTED_EDGE ( 'NONE', *, *, #18026, .F. ) ;
#17576 = ORIENTED_EDGE ( 'NONE', *, *, #4647, .F. ) ;
#17577 = CARTESIAN_POINT ( 'NONE',  ( -3.631840208645857437, -4.484949146646330931, -6.500000000000005329 ) ) ;
#17578 = VECTOR ( 'NONE', #2216, 1000.000000000000000 ) ;
#17579 = EDGE_CURVE ( 'NONE', #2052, #941, #1618, .T. ) ;
#17580 = DIRECTION ( 'NONE',  ( 0.000000000000000000, 1.000000000000000000, 1.099230717450651647E-14 ) ) ;
#17581 = CARTESIAN_POINT ( 'NONE',  ( -0.000000000000000000, 0.000000000000000000, 0.000000000000000000 ) ) ;
#17582 = ORIENTED_EDGE ( 'NONE', *, *, #16051, .T. ) ;
#17583 = CARTESIAN_POINT ( 'NONE',  ( -16.96448111170888851, 1.130229351527647585, 32.00000000000000000 ) ) ;
#17584 = CARTESIAN_POINT ( 'NONE',  ( 13.00000000000000178, -4.545788521379982683, -1.798195097860023628 ) ) ;
#17585 = ORIENTED_EDGE ( 'NONE', *, *, #13211, .T. ) ;
#17586 = DIRECTION ( 'NONE',  ( -1.000000000000000000, -0.000000000000000000, -0.000000000000000000 ) ) ;
#17587 = CIRCLE ( 'NONE', #4809, 2.524999999999994582 ) ;
#17588 = ADVANCED_FACE ( 'NONE', ( #11091 ), #18686, .F. ) ;
#17589 = CARTESIAN_POINT ( 'NONE',  ( 2.000000000000001776, 0.000000000000000000, -4.824999999999999289 ) ) ;
#17590 = DIRECTION ( 'NONE',  ( 0.000000000000000000, 0.000000000000000000, 1.000000000000000000 ) ) ;
#17591 = CARTESIAN_POINT ( 'NONE',  ( 2.257825459230520693, -26.58873630738055738, 4.993157874727710777 ) ) ;
#17592 = B_SPLINE_CURVE_WITH_KNOTS ( 'NONE', 3,
 ( #1057, #13447, #13655, #10266, #4256, #16658 ),
 .UNSPECIFIED., .F., .F.,
 ( 4, 2, 4 ),
 ( 2.032124546189621919E-07, 0.001878594002992306630, 0.003756984793529993989 ),
 .UNSPECIFIED. ) ;
#17593 = CARTESIAN_POINT ( 'NONE',  ( 22.00000000000000355, 0.000000000000000000, 32.00000000000000000 ) ) ;
#17594 = CARTESIAN_POINT ( 'NONE',  ( 2.789999999999999147, 24.44424927289185945, -0.2301004812058395077 ) ) ;
#17595 = SURFACE_STYLE_FILL_AREA ( #14198 ) ;
#17596 = EDGE_LOOP ( 'NONE', ( #15398, #8484, #850, #15088 ) ) ;
#17597 = CARTESIAN_POINT ( 'NONE',  ( 9.312499995903225525, 5.668774803599156975, 0.5958122406256377568 ) ) ;
#17598 = CARTESIAN_POINT ( 'NONE',  ( -20.63749999999999574, 0.000000000000000000, 0.000000000000000000 ) ) ;
#17599 = PRODUCT_DEFINITION_CONTEXT ( 'detailed design', #18010, 'design' ) ;
#17600 = DIRECTION ( 'NONE',  ( 0.000000000000000000, 0.000000000000000000, 1.000000000000000000 ) ) ;
#17601 = CARTESIAN_POINT ( 'NONE',  ( 10.46874999795161720, -3.632567103900500971, -3.270778111535363131 ) ) ;
#17602 = DIRECTION ( 'NONE',  ( -1.000000000000000000, 0.000000000000000000, 0.000000000000000000 ) ) ;
#17603 = AXIS2_PLACEMENT_3D ( 'NONE', #13350, #16563, #4543 ) ;
#17604 = CARTESIAN_POINT ( 'NONE',  ( -4.780397808154247308, 1.280903732194486722, -14.34374999795161543 ) ) ;
#17605 = ORIENTED_EDGE ( 'NONE', *, *, #18735, .F. ) ;
#17606 = CYLINDRICAL_SURFACE ( 'NONE', #15394, 0.9999999999999974465 ) ;
#17607 = EDGE_CURVE ( 'NONE', #1381, #3988, #383, .T. ) ;
#17608 = EDGE_CURVE ( 'NONE', #19636, #18433, #12303, .T. ) ;
#17609 = FACE_OUTER_BOUND ( 'NONE', #1656, .T. ) ;
#17610 = ORIENTED_EDGE ( 'NONE', *, *, #14969, .T. ) ;
#17611 = DIRECTION ( 'NONE',  ( -1.000000000000000000, 0.000000000000000000, 0.000000000000000000 ) ) ;
#17612 = DIRECTION ( 'NONE',  ( -0.000000000000000000, 0.000000000000000000, 1.000000000000000000 ) ) ;
#17613 = EDGE_CURVE ( 'NONE', #9421, #10348, #15692, .T. ) ;
#17614 = CARTESIAN_POINT ( 'NONE',  ( 0.02436607992776455150, -22.71065055754459650, 9.836394144775621129 ) ) ;
#17615 = DIRECTION ( 'NONE',  ( 0.000000000000000000, 0.000000000000000000, 1.000000000000000000 ) ) ;
#17616 = EDGE_LOOP ( 'NONE', ( #12435, #13609, #8045, #12826 ) ) ;
#17617 = AXIS2_PLACEMENT_3D ( 'NONE', #2229, #4943, #11349 ) ;
#17618 = AXIS2_PLACEMENT_3D ( 'NONE', #3771, #1969, #17282 ) ;
#17619 = CARTESIAN_POINT ( 'NONE',  ( 14.86923836996420434, -11.47363181547641453, 32.00000000000000000 ) ) ;
#17620 =( LENGTH_UNIT ( ) NAMED_UNIT ( * ) SI_UNIT ( .MILLI., .METRE. ) );
#17621 = CARTESIAN_POINT ( 'NONE',  ( 1.394999999999998685, 25.12109765559653596, 12.52377138324232675 ) ) ;
#17622 = AXIS2_PLACEMENT_3D ( 'NONE', #8435, #14333, #11525 ) ;
#17623 = ORIENTED_EDGE ( 'NONE', *, *, #12734, .T. ) ;
#17624 = DIRECTION ( 'NONE',  ( 0.000000000000000000, 0.000000000000000000, 1.000000000000000000 ) ) ;
#17625 = VERTEX_POINT ( 'NONE', #14189 ) ;
#17626 = APPLICATION_CONTEXT ( 'automotive_design' ) ;
#17627 = CARTESIAN_POINT ( 'NONE',  ( -2.291930025145539673, 7.842189106403748333, -0.1296323192022596493 ) ) ;
#17628 = DIRECTION ( 'NONE',  ( 0.000000000000000000, 1.000000000000000000, 0.000000000000000000 ) ) ;
#17629 = DIRECTION ( 'NONE',  ( -1.000000000000000000, 0.000000000000000000, 0.000000000000000000 ) ) ;
#17630 = CARTESIAN_POINT ( 'NONE',  ( -17.68117051311639898, -3.372863662543042818, 35.00000000000000000 ) ) ;
#17631 = ORIENTED_EDGE ( 'NONE', *, *, #15532, .T. ) ;
#17632 = DIRECTION ( 'NONE',  ( 0.000000000000000000, 0.000000000000000000, 1.000000000000000000 ) ) ;
#17633 = LINE ( 'NONE', #16035, #16830 ) ;
#17634 = TOROIDAL_SURFACE ( 'NONE', #16678, 4.200000000000000178, 0.1999999999999998723 ) ;
#17635 = ORIENTED_EDGE ( 'NONE', *, *, #353, .F. ) ;
#17636 = CIRCLE ( 'NONE', #5787, 1.000000000000004441 ) ;
#17637 = AXIS2_PLACEMENT_3D ( 'NONE', #3105, #18510, #4907 ) ;
#17638 = EDGE_CURVE ( 'NONE', #13278, #2736, #991, .T. ) ;
#17639 = DIRECTION ( 'NONE',  ( 1.000000000000000000, 0.000000000000000000, 0.000000000000000000 ) ) ;
#17640 = DIRECTION ( 'NONE',  ( 0.000000000000000000, 0.000000000000000000, 1.000000000000000000 ) ) ;
#17641 = EDGE_CURVE ( 'NONE', #14953, #17016, #12693, .T. ) ;
#17642 = ORIENTED_EDGE ( 'NONE', *, *, #5496, .T. ) ;
#17643 = CARTESIAN_POINT ( 'NONE',  ( -2.000000000000001776, 0.000000000000000000, -8.265000000000021885 ) ) ;
#17644 = CARTESIAN_POINT ( 'NONE',  ( -3.954556930911881096, -2.873153789725797935, -14.46874999795161720 ) ) ;
#17645 = FACE_BOUND ( 'NONE', #2267, .T. ) ;
#17646 = ORIENTED_EDGE ( 'NONE', *, *, #18328, .F. ) ;
#17647 = DIRECTION ( 'NONE',  ( -0.000000000000000000, -0.000000000000000000, 1.000000000000000000 ) ) ;
#17648 = AXIS2_PLACEMENT_3D ( 'NONE', #9502, #3582, #15402 ) ;
#17649 = ORIENTED_EDGE ( 'NONE', *, *, #18728, .T. ) ;
#17650 = CIRCLE ( 'NONE', #79, 9.000000000000021316 ) ;
#17651 = FILL_AREA_STYLE ('',( #18852 ) ) ;
#17652 = CIRCLE ( 'NONE', #17618, 10.00000000000000000 ) ;
#17653 = CARTESIAN_POINT ( 'NONE',  ( -5.476417968967388639, 17.43449690031536292, -32.00000000000000000 ) ) ;
#17654 = ORIENTED_EDGE ( 'NONE', *, *, #11064, .F. ) ;
#17655 = EDGE_CURVE ( 'NONE', #9505, #8042, #3214, .T. ) ;
#17656 = CARTESIAN_POINT ( 'NONE',  ( 0.7741991708318548548, -4.888101187500005551, -10.96874999795161720 ) ) ;
#17657 = CARTESIAN_POINT ( 'NONE',  ( 13.00000000000000000, -3.840809689102975710, 4.211671987713753396 ) ) ;
#17658 = FACE_OUTER_BOUND ( 'NONE', #11344, .T. ) ;
#17659 = ORIENTED_EDGE ( 'NONE', *, *, #4623, .T. ) ;
#17660 = PRESENTATION_LAYER_ASSIGNMENT (  '', '', ( #18280 ) ) ;
#17661 = EDGE_CURVE ( 'NONE', #5161, #11518, #4593, .T. ) ;
#17662 = ADVANCED_FACE ( 'NONE', ( #4788 ), #10896, .F. ) ;
#17663 = CARTESIAN_POINT ( 'NONE',  ( 4.888101187500000222, -3.413342815706642518E-14, -6.843749997951615427 ) ) ;
#17664 = AXIS2_PLACEMENT_3D ( 'NONE', #12377, #12578, #7763 ) ;
#17665 = ORIENTED_EDGE ( 'NONE', *, *, #816, .F. ) ;
#17666 = AXIS2_PLACEMENT_3D ( 'NONE', #13743, #18057, #10649 ) ;
#17667 = VECTOR ( 'NONE', #3036, 1000.000000000000000 ) ;
#17668 = DIRECTION ( 'NONE',  ( 1.000000000000000000, 0.000000000000000000, 0.000000000000000000 ) ) ;
#17669 = COLOUR_RGB ( '', 0.40784314, 0.44705882, 0.49803922) ;
#17670 = CARTESIAN_POINT ( 'NONE',  ( 6.000593838912648081, -0.002144393866035136480, 5.699999596629369059 ) ) ;
#17671 = ORIENTED_EDGE ( 'NONE', *, *, #7191, .T. ) ;
#17672 = CARTESIAN_POINT ( 'NONE',  ( -4.780397808154273953, -1.280903732194386579, -9.343749997951615427 ) ) ;
#17673 = CARTESIAN_POINT ( 'NONE',  ( 17.96448111170888851, 1.130229351527639148, 32.00000000000000000 ) ) ;
#17674 = ADVANCED_FACE ( 'NONE', ( #9501 ), #14393, .T. ) ;
#17675 = ORIENTED_EDGE ( 'NONE', *, *, #8754, .F. ) ;
#17676 = EDGE_LOOP ( 'NONE', ( #857, #7659, #10705, #996 ) ) ;
#17677 = DIRECTION ( 'NONE',  ( 0.000000000000000000, 0.000000000000000000, -1.000000000000000000 ) ) ;
#17678 = AXIS2_PLACEMENT_3D ( 'NONE', #8163, #573, #6644 ) ;
#17679 = CARTESIAN_POINT ( 'NONE',  ( 0.000000000000000000, 0.000000000000000000, 0.000000000000000000 ) ) ;
#17680 = DIRECTION ( 'NONE',  ( 0.000000000000000000, 0.000000000000000000, 1.000000000000000000 ) ) ;
#17681 = ORIENTED_EDGE ( 'NONE', *, *, #15285, .T. ) ;
#17682 = DIRECTION ( 'NONE',  ( 1.000000000000000000, 0.000000000000000000, -0.000000000000000000 ) ) ;
#17683 = B_SPLINE_CURVE_WITH_KNOTS ( 'NONE', 3,
 ( #6752, #10172, #3663, #9788 ),
 .UNSPECIFIED., .F., .F.,
 ( 4, 4 ),
 ( 0.003263275852154239043, 0.003756984793529996591 ),
 .UNSPECIFIED. ) ;
#17684 = CARTESIAN_POINT ( 'NONE',  ( -9.580134541264520465, -14.56230589874905235, 32.00000000000000000 ) ) ;
#17685 = EDGE_LOOP ( 'NONE', ( #17781, #4319, #15158, #1687, #15722, #4406 ) ) ;
#17686 = DIRECTION ( 'NONE',  ( 0.000000000000000000, 0.000000000000000000, 1.000000000000000000 ) ) ;
#17687 = LINE ( 'NONE', #14690, #1663 ) ;
#17688 = DIRECTION ( 'NONE',  ( 0.000000000000000000, 0.000000000000000000, -1.000000000000000000 ) ) ;
#17689 = CARTESIAN_POINT ( 'NONE',  ( 11.84374999795161365, 2.444050593749991229, 4.233219804643887585 ) ) ;
#17690 = PRODUCT ( 'Internal Brake Shoe', 'Internal Brake Shoe', '', ( #15558 ) ) ;
#17691 = CARTESIAN_POINT ( 'NONE',  ( -30.00000000000000000, 4.400000000000000355, 0.000000000000000000 ) ) ;
#17692 = CARTESIAN_POINT ( 'NONE',  ( 2.500000000000002220, 0.000000000000000000, 0.000000000000000000 ) ) ;
#17693 = AXIS2_PLACEMENT_3D ( 'NONE', #15694, #4696, #6465 ) ;
#17694 = ORIENTED_EDGE ( 'NONE', *, *, #13356, .T. ) ;
#17695 = DIRECTION ( 'NONE',  ( 0.000000000000000000, 0.000000000000000000, 1.000000000000000000 ) ) ;
#17696 = FACE_OUTER_BOUND ( 'NONE', #9766, .T. ) ;
#17697 = CARTESIAN_POINT ( 'NONE',  ( 4.150607464521812062, 2.695436003842704764, -8.343749997951611874 ) ) ;
#17698 = CARTESIAN_POINT ( 'NONE',  ( 2.291930025145539229, -7.842189106403761656, -0.1296323192022672544 ) ) ;
#17699 =( GEOMETRIC_REPRESENTATION_CONTEXT ( 3 ) GLOBAL_UNCERTAINTY_ASSIGNED_CONTEXT ( ( #603 ) ) GLOBAL_UNIT_ASSIGNED_CONTEXT ( ( #7664, #9184, #7461 ) ) REPRESENTATION_CONTEXT ( 'NONE', 'WORKASPACE' ) );
#17700 = AXIS2_PLACEMENT_3D ( 'NONE', #15381, #18085, #11982 ) ;
#17701 = CARTESIAN_POINT ( 'NONE',  ( 2.873153789725825025, 3.954556930911862000, -13.84374999795161543 ) ) ;
#17702 = EDGE_CURVE ( 'NONE', #6503, #809, #18885, .T. ) ;
#17703 = ORIENTED_EDGE ( 'NONE', *, *, #4345, .F. ) ;
#17704 = DIRECTION ( 'NONE',  ( -1.000000000000000000, 0.000000000000000000, 0.000000000000000000 ) ) ;
#17705 = CARTESIAN_POINT ( 'NONE',  ( 2.790000000000077751, 12.51293083811798645, 20.85287692521934488 ) ) ;
#17706 = ORIENTED_EDGE ( 'NONE', *, *, #5459, .F. ) ;
#17707 = B_SPLINE_CURVE_WITH_KNOTS ( 'NONE', 3,
 ( #6323, #7634, #12447, #3736, #2134, #9549 ),
 .UNSPECIFIED., .F., .F.,
 ( 4, 2, 4 ),
 ( 4.462636732872785396E-07, 0.001879885066975069564, 0.003759323870276851630 ),
 .UNSPECIFIED. ) ;
#17708 =( NAMED_UNIT ( * ) PLANE_ANGLE_UNIT ( ) SI_UNIT ( $, .RADIAN. ) );
#17709 = AXIS2_PLACEMENT_3D ( 'NONE', #3064, #1378, #4470 ) ;
#17710 = DIRECTION ( 'NONE',  ( 0.000000000000000000, 0.000000000000000000, -1.000000000000000000 ) ) ;
#17711 = DIRECTION ( 'NONE',  ( 0.000000000000000000, 0.000000000000000000, 1.000000000000000000 ) ) ;
#17712 = CARTESIAN_POINT ( 'NONE',  ( 91.50000000000000000, 0.000000000000000000, 0.000000000000000000 ) ) ;
#17713 = ORIENTED_EDGE ( 'NONE', *, *, #17996, .T. ) ;
#17714 = AXIS2_PLACEMENT_3D ( 'NONE', #5550, #7136, #17765 ) ;
#17715 = CARTESIAN_POINT ( 'NONE',  ( -2.000000000000000000, -2.000000000000001776, 41.99999999999999289 ) ) ;
#17716 = DIRECTION ( 'NONE',  ( 0.000000000000000000, 0.000000000000000000, 1.000000000000000000 ) ) ;
#17717 = EDGE_CURVE ( 'NONE', #18417, #2730, #7314, .T. ) ;
#17718 = DIRECTION ( 'NONE',  ( -0.000000000000000000, -0.000000000000000000, 1.000000000000000000 ) ) ;
#17719 = ORIENTED_EDGE ( 'NONE', *, *, #13778, .T. ) ;
#17720 = CARTESIAN_POINT ( 'NONE',  ( 10.31249999590322552, -5.207209108562803834, -2.318398865532109721 ) ) ;
#17721 = EDGE_LOOP ( 'NONE', ( #5704, #12567 ) ) ;
#17722 = CARTESIAN_POINT ( 'NONE',  ( 0.7592463941534229876, -3.797885586973023475, -27.31305418910213234 ) ) ;
#17723 = AXIS2_PLACEMENT_3D ( 'NONE', #16314, #913, #14911 ) ;
#17724 = B_SPLINE_CURVE_WITH_KNOTS ( 'NONE', 3,
 ( #9387, #15292, #18384, #4973 ),
 .UNSPECIFIED., .F., .F.,
 ( 4, 4 ),
 ( 0.005258139959819237326, 0.005948405594583419317 ),
 .UNSPECIFIED. ) ;
#17725 = DIRECTION ( 'NONE',  ( -1.000000000000000000, 0.000000000000000000, 0.000000000000000000 ) ) ;
#17726 = CARTESIAN_POINT ( 'NONE',  ( -2.000000000000001776, 0.000000000000000000, -5.200000000000000178 ) ) ;
#17727 = CARTESIAN_POINT ( 'NONE',  ( 3.350375938067096548, 4.611396867937201272, -13.00000000000000533 ) ) ;
#17728 = ADVANCED_FACE ( 'NONE', ( #17491 ), #3780, .F. ) ;
#17729 = ORIENTED_EDGE ( 'NONE', *, *, #4351, .F. ) ;
#17730 = FACE_BOUND ( 'NONE', #2837, .T. ) ;
#17731 = DIRECTION ( 'NONE',  ( -1.000000000000000000, -0.000000000000000000, -0.000000000000000000 ) ) ;
#17732 = AXIS2_PLACEMENT_3D ( 'NONE', #814, #6791, #9926 ) ;
#17733 = ORIENTED_EDGE ( 'NONE', *, *, #8123, .T. ) ;
#17734 = CARTESIAN_POINT ( 'NONE',  ( 2.789999999999999147, 23.17675759782029843, 7.772527002114834715 ) ) ;
#17735 = DIRECTION ( 'NONE',  ( 0.000000000000000000, 0.000000000000000000, 1.000000000000000000 ) ) ;
#17736 = ORIENTED_EDGE ( 'NONE', *, *, #19542, .F. ) ;
#17737 = CARTESIAN_POINT ( 'NONE',  ( -7.937500000000000000, -0.7744039358429345432, 6.268043809681820044E-17 ) ) ;
#17738 = CARTESIAN_POINT ( 'NONE',  ( 6.000000000000005329, 5.700000000000001954, 0.000000000000000000 ) ) ;
#17739 = CARTESIAN_POINT ( 'NONE',  ( 6.968749997951614539, 0.7741991708318887166, -4.888101187500000222 ) ) ;
#17740 = VERTEX_POINT ( 'NONE', #5174 ) ;
#17741 = EDGE_CURVE ( 'NONE', #9467, #11508, #686, .T. ) ;
#17742 = LINE ( 'NONE', #2338, #14830 ) ;
#17743 = CARTESIAN_POINT ( 'NONE',  ( -16.96448111170888851, 1.130229351527647585, 35.00000000000000000 ) ) ;
#17744 = AXIS2_PLACEMENT_3D ( 'NONE', #18887, #9701, #489 ) ;
#17745 = ORIENTED_EDGE ( 'NONE', *, *, #3164, .F. ) ;
#17746 = AXIS2_PLACEMENT_3D ( 'NONE', #1570, #4279, #1379 ) ;
#17747 = CARTESIAN_POINT ( 'NONE',  ( 1.039999999999995817, -27.76164181293048472, -4.147968289691575272 ) ) ;
#17748 = CARTESIAN_POINT ( 'NONE',  ( -4.465502636338010589, 1.988169868018623720, -14.46874999795161720 ) ) ;
#17749 = ORIENTED_EDGE ( 'NONE', *, *, #2669, .T. ) ;
#17750 = CARTESIAN_POINT ( 'NONE',  ( -4.476417968967385974, 17.43449690031536292, -32.00000000000000000 ) ) ;
#17751 = CARTESIAN_POINT ( 'NONE',  ( 9.000000000000000000, 0.000000000000000000, 29.00000000000000355 ) ) ;
#17752 = EDGE_CURVE ( 'NONE', #5897, #4232, #4832, .T. ) ;
#17753 = DIRECTION ( 'NONE',  ( 0.000000000000000000, 0.000000000000000000, 1.000000000000000000 ) ) ;
#17754 = VERTEX_POINT ( 'NONE', #19447 ) ;
#17755 = EDGE_CURVE ( 'NONE', #9521, #3237, #18263, .T. ) ;
#17756 = CARTESIAN_POINT ( 'NONE',  ( 1.749999999999998002, -4.147968289691484678, 27.76164181293050603 ) ) ;
#17757 = CIRCLE ( 'NONE', #2735, 0.9999999999999974465 ) ;
#17758 = EDGE_LOOP ( 'NONE', ( #864, #13721, #13223, #8270 ) ) ;
#17759 = AXIS2_PLACEMENT_3D ( 'NONE', #12984, #15982, #3867 ) ;
#17760 = B_SPLINE_CURVE_WITH_KNOTS ( 'NONE', 3,
 ( #15480, #12379, #18571, #10873, #15875, #17375 ),
 .UNSPECIFIED., .F., .F.,
 ( 4, 2, 4 ),
 ( 2.032124546189621919E-07, 0.001878594002992309232, 0.003756984793529999193 ),
 .UNSPECIFIED. ) ;
#17761 = EDGE_CURVE ( 'NONE', #14183, #16193, #7049, .T. ) ;
#17762 = DIRECTION ( 'NONE',  ( -1.000000000000000000, 0.000000000000000000, 0.000000000000000000 ) ) ;
#17763 = CARTESIAN_POINT ( 'NONE',  ( -4.200000000000001954, 5.143516556418886872E-16, -6.000000000000005329 ) ) ;
#17764 = ORIENTED_EDGE ( 'NONE', *, *, #12302, .F. ) ;
#17765 = DIRECTION ( 'NONE',  ( 0.000000000000000000, 0.000000000000000000, 1.000000000000000000 ) ) ;
#17766 = PRESENTATION_STYLE_ASSIGNMENT (( #5263 ) ) ;
#17767 = ADVANCED_FACE ( 'NONE', ( #9901 ), #10363, .F. ) ;
#17768 = SURFACE_STYLE_FILL_AREA ( #2451 ) ;
#17769 = ORIENTED_EDGE ( 'NONE', *, *, #11530, .F. ) ;
#17770 = EDGE_LOOP ( 'NONE', ( #10492, #13367 ) ) ;
#17771 = CARTESIAN_POINT ( 'NONE',  ( -11.00000000000000355, -4.898587196589412829E-16, 0.000000000000000000 ) ) ;
#17772 = CIRCLE ( 'NONE', #10747, 1.000000000000000000 ) ;
#17773 = LINE ( 'NONE', #4067, #14304 ) ;
#17774 = CIRCLE ( 'NONE', #8185, 9.000000000000001776 ) ;
#17775 = ORIENTED_EDGE ( 'NONE', *, *, #1956, .T. ) ;
#17776 = ADVANCED_FACE ( 'NONE', ( #4251 ), #592, .T. ) ;
#17777 = DIRECTION ( 'NONE',  ( -1.000000000000000000, 0.000000000000000000, 0.000000000000000000 ) ) ;
#17778 = ORIENTED_EDGE ( 'NONE', *, *, #19472, .T. ) ;
#17779 = CARTESIAN_POINT ( 'NONE',  ( -12.32184790671639085, 13.12143529358541549, -32.00000000000000000 ) ) ;
#17780 = CARTESIAN_POINT ( 'NONE',  ( 13.00000000000000178, -4.568735188514048140, -1.737869959597788672 ) ) ;
#17781 = ORIENTED_EDGE ( 'NONE', *, *, #17414, .F. ) ;
#17782 = CARTESIAN_POINT ( 'NONE',  ( 16.68117051311640253, -3.372863662543048591, -32.00000000000000000 ) ) ;
#17783 = ADVANCED_FACE ( 'NONE', ( #3679 ), #11754, .F. ) ;
#17784 = CIRCLE ( 'NONE', #18101, 1.000000000000002665 ) ;
#17785 = AXIS2_PLACEMENT_3D ( 'NONE', #18299, #4687, #12298 ) ;
#17786 = CARTESIAN_POINT ( 'NONE',  ( -90.00000000000000000, 1.012170579495290078E-15, 8.265000000000021885 ) ) ;
#17787 = DIRECTION ( 'NONE',  ( -1.000000000000000000, 0.000000000000000000, 0.000000000000000000 ) ) ;
#17788 = CARTESIAN_POINT ( 'NONE',  ( 13.00000000000000178, -0.7793280607714923036, -4.825575716215948496 ) ) ;
#17789 = DIRECTION ( 'NONE',  ( -1.000000000000000000, -0.000000000000000000, -0.000000000000000000 ) ) ;
#17790 = PRESENTATION_STYLE_ASSIGNMENT (( #9908 ) ) ;
#17791 = DIRECTION ( 'NONE',  ( -1.000000000000000000, 0.000000000000000000, 0.000000000000000000 ) ) ;
#17792 = ORIENTED_EDGE ( 'NONE', *, *, #15745, .F. ) ;
#17793 = DIRECTION ( 'NONE',  ( -1.000000000000000000, -0.000000000000000000, -0.000000000000000000 ) ) ;
#17794 = DIRECTION ( 'NONE',  ( 1.000000000000000000, 0.000000000000000000, 0.000000000000000000 ) ) ;
#17795 = UNCERTAINTY_MEASURE_WITH_UNIT (LENGTH_MEASURE( 1.000000000000000082E-05 ), #9346, 'distance_accuracy_value', 'NONE');
#17796 = LINE ( 'NONE', #10496, #7029 ) ;
#17797 =( BOUNDED_CURVE ( )  B_SPLINE_CURVE ( 2, ( #12491, #379, #18488, #3283, #10989, #6362, #6661, #9396, #17094, #3385, #8077, #12787, #9496, #15593, #15397 ),
 .UNSPECIFIED., .F., .F. ) 
 B_SPLINE_CURVE_WITH_KNOTS ( ( 3, 2, 2, 2, 2, 2, 2, 3 ),
 ( 0.000000000000000000, 0.05000000000000000278, 0.1000000000000000056, 0.1499999999999999944, 0.2000000000000000111, 0.2500000000000000000, 0.2999999999999999889, 0.3078686208676164604 ),
 .UNSPECIFIED. ) 
 CURVE ( )  GEOMETRIC_REPRESENTATION_ITEM ( )  RATIONAL_B_SPLINE_CURVE ( ( 1.000000000000000000, 0.9876883405951377704, 1.000000000000000000, 0.9876883405951377704, 1.000000000000000000, 0.9876883405951377704, 1.000000000000000000, 0.9876883405951377704, 1.000000000000000000, 0.9876883405951377704, 1.000000000000000000, 0.9876883405951377704, 1.000000000000000000, 0.9980624843978382899, 0.9967347918236166837 ) ) 
 REPRESENTATION_ITEM ( '' )  );
#17798 = CARTESIAN_POINT ( 'NONE',  ( 1.988169868018562880, -4.465502636338038123, -13.46874999795161543 ) ) ;
#17799 = AXIS2_PLACEMENT_3D ( 'NONE', #19333, #11640, #4969 ) ;
#17800 = CARTESIAN_POINT ( 'NONE',  ( -4.465502636338010589, 1.988169868018623720, -14.84374999795161543 ) ) ;
#17801 = AXIS2_PLACEMENT_3D ( 'NONE', #10689, #16798, #1483 ) ;
#17802 = EDGE_LOOP ( 'NONE', ( #10216, #7307, #13333, #12042 ) ) ;
#17803 = DIRECTION ( 'NONE',  ( 0.000000000000000000, 0.000000000000000000, 1.000000000000000000 ) ) ;
#17804 = CARTESIAN_POINT ( 'NONE',  ( 13.00000000000000178, 0.000000000000000000, 0.000000000000000000 ) ) ;
#17805 = ORIENTED_EDGE ( 'NONE', *, *, #2864, .F. ) ;
#17806 = CYLINDRICAL_SURFACE ( 'NONE', #2707, 5.200000000000000178 ) ;
#17807 = EDGE_CURVE ( 'NONE', #201, #5154, #8753, .T. ) ;
#17808 = CARTESIAN_POINT ( 'NONE',  ( 2.718184743034449014, 5.344212458769360907, 24.78695292654923676 ) ) ;
#17809 = DIRECTION ( 'NONE',  ( 1.000000000000000000, 0.000000000000000000, 0.000000000000000000 ) ) ;
#17810 = DIRECTION ( 'NONE',  ( -1.000000000000000000, -0.000000000000000000, -0.000000000000000000 ) ) ;
#17811 = ORIENTED_EDGE ( 'NONE', *, *, #16098, .F. ) ;
#17812 = CIRCLE ( 'NONE', #11102, 2.524999999999995914 ) ;
#17813 = FACE_OUTER_BOUND ( 'NONE', #7551, .T. ) ;
#17814 = DIRECTION ( 'NONE',  ( 0.000000000000000000, 0.000000000000000000, 1.000000000000000000 ) ) ;
#17815 = EDGE_CURVE ( 'NONE', #10991, #9264, #1246, .T. ) ;
#17816 = CIRCLE ( 'NONE', #19407, 4.000000000000000000 ) ;
#17817 =( NAMED_UNIT ( * ) SI_UNIT ( $, .STERADIAN. ) SOLID_ANGLE_UNIT ( ) );
#17818 = EDGE_LOOP ( 'NONE', ( #15910, #18985 ) ) ;
#17819 = CARTESIAN_POINT ( 'NONE',  ( 2.765633920072234631, 5.391175441198615914, 24.15498966839965078 ) ) ;
#17820 = ORIENTED_EDGE ( 'NONE', *, *, #14344, .F. ) ;
#17821 = CARTESIAN_POINT ( 'NONE',  ( 0.0003207540509381473352, -20.70663861606275447, -12.51925356660783528 ) ) ;
#17822 = CARTESIAN_POINT ( 'NONE',  ( 4.762500000000000178, 0.000000000000000000, -6.527800000000000047 ) ) ;
#17823 = CARTESIAN_POINT ( 'NONE',  ( -20.63749999999999574, 0.000000000000000000, -8.000000000000000000 ) ) ;
#17824 = EDGE_CURVE ( 'NONE', #271, #19757, #19543, .T. ) ;
#17825 = CARTESIAN_POINT ( 'NONE',  ( -19.00000000000000355, -4.898587196589412829E-16, 0.000000000000000000 ) ) ;
#17826 = VERTEX_POINT ( 'NONE', #16559 ) ;
#17827 = CARTESIAN_POINT ( 'NONE',  ( -0.5109457054262123155, -4.861323657744403448, -8.843749997951615427 ) ) ;
#17828 = DIRECTION ( 'NONE',  ( 0.000000000000000000, 1.000000000000000000, -1.224646799147353207E-16 ) ) ;
#17829 = AXIS2_PLACEMENT_3D ( 'NONE', #7359, #17998, #16692 ) ;
#17830 = VERTEX_POINT ( 'NONE', #9350 ) ;
#17831 = CARTESIAN_POINT ( 'NONE',  ( 2.999999999999998224, -3.950217066951263956, -3.681818181818183877 ) ) ;
#17832 = CARTESIAN_POINT ( 'NONE',  ( 3.350375938067065462, -4.611396867937225252, -10.31249999590322552 ) ) ;
#17833 = ORIENTED_EDGE ( 'NONE', *, *, #8191, .F. ) ;
#17834 = CARTESIAN_POINT ( 'NONE',  ( 4.781284448697194378, 1.016293382781411792, -12.46874999795161543 ) ) ;
#17835 = DIRECTION ( 'NONE',  ( 0.000000000000000000, 0.000000000000000000, 1.000000000000000000 ) ) ;
#17836 = FACE_BOUND ( 'NONE', #6925, .T. ) ;
#17837 = EDGE_CURVE ( 'NONE', #18641, #1940, #6105, .T. ) ;
#17838 = ORIENTED_EDGE ( 'NONE', *, *, #531, .T. ) ;
#17839 = CARTESIAN_POINT ( 'NONE',  ( 2.790000000000077307, 23.69897269326684963, -5.456611084821608948 ) ) ;
#17840 = VERTEX_POINT ( 'NONE', #8949 ) ;
#17842 = CARTESIAN_POINT ( 'NONE',  ( 12.99999999999969624, 1.390454305316116246, 5.264438301130793363 ) ) ;
#17841 = AXIS2_PLACEMENT_3D ( 'NONE', #76, #19776, #15584 ) ;
#17843 = EDGE_LOOP ( 'NONE', ( #12838, #7753 ) ) ;
#17844 = CARTESIAN_POINT ( 'NONE',  ( 6.468749997951615427, 4.233219804643871598, 2.444050593750020095 ) ) ;
#17845 = FACE_OUTER_BOUND ( 'NONE', #1313, .T. ) ;
#17846 = DIRECTION ( 'NONE',  ( -0.000000000000000000, -0.000000000000000000, 1.000000000000000000 ) ) ;
#17847 = CARTESIAN_POINT ( 'NONE',  ( 2.000000000000001776, 0.000000000000000000, 0.000000000000000000 ) ) ;
#17848 = CARTESIAN_POINT ( 'NONE',  ( 2.789999999999999147, -24.04302995059964587, -1.991882183130548878 ) ) ;
#17849 = CARTESIAN_POINT ( 'NONE',  ( -36.00000000000000000, -2.311115933264683024E-31, 0.000000000000000000 ) ) ;
#17850 = ORIENTED_EDGE ( 'NONE', *, *, #19741, .F. ) ;
#17851 = CARTESIAN_POINT ( 'NONE',  ( 0.07186815222487989707, 5.344160105508701797, 24.78765742476140943 ) ) ;
#17852 = EDGE_CURVE ( 'NONE', #17485, #6807, #15051, .T. ) ;
#17853 = PRODUCT_DEFINITION_SHAPE ( 'NONE', 'NONE',  #19797 ) ;
#17854 = AXIS2_PLACEMENT_3D ( 'NONE', #1758, #16777, #13865 ) ;
#17855 = VERTEX_POINT ( 'NONE', #38 ) ;
#17856 = CARTESIAN_POINT ( 'NONE',  ( 17.11901729331276556, 5.562305898749055011, 32.00000000000000000 ) ) ;
#17857 = EDGE_CURVE ( 'NONE', #18527, #8351, #14382, .T. ) ;
#17858 = DIRECTION ( 'NONE',  ( 0.000000000000000000, 1.000000000000000000, -1.224646799147353207E-16 ) ) ;
#17859 = DIRECTION ( 'NONE',  ( 0.000000000000000000, 0.000000000000000000, 1.000000000000000000 ) ) ;
#17860 = PRESENTATION_LAYER_ASSIGNMENT (  '', '', ( #11469 ) ) ;
#17861 = B_SPLINE_CURVE_WITH_KNOTS ( 'NONE', 3,
 ( #2604, #13513, #4409, #8715, #15019, #19616 ),
 .UNSPECIFIED., .F., .F.,
 ( 4, 2, 4 ),
 ( 1.979325885420663221E-07, 0.001878588715165609505, 0.003756979497742676637 ),
 .UNSPECIFIED. ) ;
#17862 = CARTESIAN_POINT ( 'NONE',  ( -5.209999999999999964, 0.000000000000000000, 0.000000000000000000 ) ) ;
#17863 = ORIENTED_EDGE ( 'NONE', *, *, #5198, .F. ) ;
#17864 = CYLINDRICAL_SURFACE ( 'NONE', #17714, 28.06981291497571362 ) ;
#17865 = DIRECTION ( 'NONE',  ( -0.000000000000000000, -0.000000000000000000, -1.000000000000000000 ) ) ;
#17866 = CARTESIAN_POINT ( 'NONE',  ( 1.773574444220693103, -4.620319390059841602, -6.968749997951614539 ) ) ;
#17867 = ORIENTED_EDGE ( 'NONE', *, *, #6685, .T. ) ;
#17868 = ORIENTED_EDGE ( 'NONE', *, *, #13159, .F. ) ;
#17869 = CARTESIAN_POINT ( 'NONE',  ( 1.039999999999996705, -19.67366047555515252, -20.02152543075367319 ) ) ;
#17870 = CIRCLE ( 'NONE', #16754, 6.735000000000022524 ) ;
#17871 = FACE_OUTER_BOUND ( 'NONE', #2261, .T. ) ;
#17872 = EDGE_LOOP ( 'NONE', ( #16262, #7846, #14175, #11898, #5139, #14044 ) ) ;
#17873 = MECHANICAL_DESIGN_GEOMETRIC_PRESENTATION_REPRESENTATION (  '', ( #11802 ), #1265 ) ;
#17874 = CARTESIAN_POINT ( 'NONE',  ( -1.310841663519413114, 0.000000000000000000, 0.000000000000000000 ) ) ;
#17875 = CARTESIAN_POINT ( 'NONE',  ( -2.000000000000001776, 0.000000000000000000, 0.000000000000000000 ) ) ;
#17876 = ORIENTED_EDGE ( 'NONE', *, *, #1237, .F. ) ;
#17877 = CARTESIAN_POINT ( 'NONE',  ( 2.789999999999999147, 24.15498966839963302, 5.391175441198700291 ) ) ;
#17878 = CARTESIAN_POINT ( 'NONE',  ( 111.3234999999999957, 0.000000000000000000, 0.000000000000000000 ) ) ;
#17879 = ORIENTED_EDGE ( 'NONE', *, *, #2082, .T. ) ;
#17880 = CARTESIAN_POINT ( 'NONE',  ( 0.000000000000000000, 0.000000000000000000, 0.000000000000000000 ) ) ;
#17881 = EDGE_CURVE ( 'NONE', #4586, #5154, #1641, .T. ) ;
#17882 = CARTESIAN_POINT ( 'NONE',  ( 89.62500000000000000, 0.000000000000000000, 4.000000000000000000 ) ) ;
#17883 = CARTESIAN_POINT ( 'NONE',  ( 14.81249999590322552, 4.080749450109650844, 4.080749450109649956 ) ) ;
#17884 = CARTESIAN_POINT ( 'NONE',  ( 12.92161831991541554, -0.8983569717628844264, -4.806352606718993670 ) ) ;
#17885 = ADVANCED_FACE ( 'NONE', ( #12154 ), #4641, .T. ) ;
#17886 = VECTOR ( 'NONE', #16847, 1000.000000000000000 ) ;
#17887 = CYLINDRICAL_SURFACE ( 'NONE', #13970, 4.200000000000001066 ) ;
#17888 =( NAMED_UNIT ( * ) SI_UNIT ( $, .STERADIAN. ) SOLID_ANGLE_UNIT ( ) );
#17889 = CONICAL_SURFACE ( 'NONE', #8632, 6.543750000000017941, 0.3653297453805220418 ) ;
#17890 = LINE ( 'NONE', #13193, #10944 ) ;
#17891 = ORIENTED_EDGE ( 'NONE', *, *, #11417, .T. ) ;
#17892 = DIRECTION ( 'NONE',  ( 0.000000000000000000, 0.000000000000000000, 1.000000000000000000 ) ) ;
#17893 = CARTESIAN_POINT ( 'NONE',  ( 1.800000000000000044, 9.552245033349356544E-16, 7.800000000000000711 ) ) ;
#17894 = DIRECTION ( 'NONE',  ( -1.000000000000000000, -0.000000000000000000, 0.000000000000000000 ) ) ;
#17895 = EDGE_CURVE ( 'NONE', #13659, #18587, #58, .T. ) ;
#17896 = CARTESIAN_POINT ( 'NONE',  ( 3.632567103900546712, 3.270778111535313837, -7.468749997951615427 ) ) ;
#17897 = DIRECTION ( 'NONE',  ( 1.000000000000000000, 0.000000000000000000, 0.000000000000000000 ) ) ;
#17898 = EDGE_LOOP ( 'NONE', ( #2018, #11669, #17092, #12530, #1157, #729 ) ) ;
#17899 = CARTESIAN_POINT ( 'NONE',  ( 8.671566133830875600, 15.77352024078954784, 32.00000000000000000 ) ) ;
#17900 = CARTESIAN_POINT ( 'NONE',  ( -2.000000000000000000, 1.999999999999998224, 37.99999999999999289 ) ) ;
#17901 = EDGE_CURVE ( 'NONE', #14216, #10239, #3871, .T. ) ;
#17902 = AXIS2_PLACEMENT_3D ( 'NONE', #18120, #15317, #15706 ) ;
#17903 = ORIENTED_EDGE ( 'NONE', *, *, #5543, .T. ) ;
#17904 = LINE ( 'NONE', #7478, #3363 ) ;
#17905 = EDGE_CURVE ( 'NONE', #18333, #14047, #3231, .T. ) ;
#17906 = VECTOR ( 'NONE', #2142, 1000.000000000000114 ) ;
#17907 = DIRECTION ( 'NONE',  ( 1.000000000000000000, 0.000000000000000000, 0.000000000000000000 ) ) ;
#17908 = CARTESIAN_POINT ( 'NONE',  ( 0.02436607992776758727, 24.15498966839963302, 5.391175441198700291 ) ) ;
#17909 = EDGE_LOOP ( 'NONE', ( #8090, #13961 ) ) ;
#17910 = DIRECTION ( 'NONE',  ( -0.000000000000000000, -0.000000000000000000, 1.000000000000000000 ) ) ;
#17911 = FILL_AREA_STYLE_COLOUR ( '', #12891 ) ;
#17912 = CARTESIAN_POINT ( 'NONE',  ( 4.942249507334556036, -0.2590123213421313686, -10.34374999795161543 ) ) ;
#17913 = CARTESIAN_POINT ( 'NONE',  ( -0.5109457054261112852, 4.861323657744413218, -14.84374999795161543 ) ) ;
#17914 = EDGE_LOOP ( 'NONE', ( #9132, #4906, #3121, #2326 ) ) ;
#17915 =( BOUNDED_SURFACE ( )  B_SPLINE_SURFACE ( 1, 2, ( 
 ( #18004, #16499, #8893, #1288, #7365, #13487, #18097, #2877, #4387, #1393, #9493, #4977, #14079, #15786, #1971, #3381, #18485 ),
 ( #9393, #18391, #12685, #4881, #17091, #18583, #4781, #10788, #6359, #83, #3477, #4684, #13988, #15684, #1686, #15393, #3570 ) ),
 .UNSPECIFIED., .F., .F., .F. ) 
 B_SPLINE_SURFACE_WITH_KNOTS ( ( 2, 2 ),
 ( 3, 2, 2, 2, 2, 2, 2, 2, 3 ),
 ( 0.000000000000000000, 1.000000000000000000 ),
 ( 0.000000000000000000, 0.05000000000000000278, 0.1000000000000000056, 0.1499999999999999944, 0.2000000000000000111, 0.2500000000000000000, 0.2999999999999999889, 0.3499999999999999778, 0.4000000000000000222 ),
 .UNSPECIFIED. ) 
 GEOMETRIC_REPRESENTATION_ITEM ( )  RATIONAL_B_SPLINE_SURFACE ( (
 ( 1.000000000000000000, 0.9876883405951377704, 1.000000000000000000, 0.9876883405951377704, 1.000000000000000000, 0.9876883405951377704, 1.000000000000000000, 0.9876883405951377704, 1.000000000000000000, 0.9876883405951377704, 1.000000000000000000, 0.9876883405951377704, 1.000000000000000000, 0.9876883405951377704, 1.000000000000000000, 0.9876883405951377704, 1.000000000000000000),
 ( 1.000000000000000000, 0.9876883405951377704, 1.000000000000000000, 0.9876883405951377704, 1.000000000000000000, 0.9876883405951377704, 1.000000000000000000, 0.9876883405951377704, 1.000000000000000000, 0.9876883405951377704, 1.000000000000000000, 0.9876883405951377704, 1.000000000000000000, 0.9876883405951377704, 1.000000000000000000, 0.9876883405951377704, 1.000000000000000000) ) ) 
 REPRESENTATION_ITEM ( '' )  SURFACE ( )  );
#17916 = CYLINDRICAL_SURFACE ( 'NONE', #5031, 28.06981291497571362 ) ;
#17917 = ORIENTED_EDGE ( 'NONE', *, *, #10476, .F. ) ;
#17918 = VECTOR ( 'NONE', #11190, 1000.000000000000000 ) ;
#17919 =( REPRESENTATION_RELATIONSHIP ('NONE','NONE', #18211, #15643 ) REPRESENTATION_RELATIONSHIP_WITH_TRANSFORMATION ( #11360 )SHAPE_REPRESENTATION_RELATIONSHIP( ) );
#17920 =( GEOMETRIC_REPRESENTATION_CONTEXT ( 3 ) GLOBAL_UNCERTAINTY_ASSIGNED_CONTEXT ( ( #4186 ) ) GLOBAL_UNIT_ASSIGNED_CONTEXT ( ( #14912, #12011, #17817 ) ) REPRESENTATION_CONTEXT ( 'NONE', 'WORKASPACE' ) );
#17921 = DIRECTION ( 'NONE',  ( -1.000000000000000000, -0.000000000000000000, -0.000000000000000000 ) ) ;
#17922 = CARTESIAN_POINT ( 'NONE',  ( 8.968749997951611874, 3.499494075959816541, -3.499494075959816541 ) ) ;
#17923 = EDGE_CURVE ( 'NONE', #6659, #5646, #18543, .T. ) ;
#17924 = CARTESIAN_POINT ( 'NONE',  ( 6.656249997951614539, -3.413342815706642518E-14, 4.888101187500000222 ) ) ;
#17925 = CARTESIAN_POINT ( 'NONE',  ( -2.620002426024544473, 5.142044285764750811, -9.500000000000005329 ) ) ;
#17926 = ORIENTED_EDGE ( 'NONE', *, *, #9817, .T. ) ;
#17927 = CARTESIAN_POINT ( 'NONE',  ( -1.280903732194487166, -4.780397808154247308, -8.968749997951611874 ) ) ;
#17928 = CARTESIAN_POINT ( 'NONE',  ( 111.3234999999999957, 0.000000000000000000, 0.000000000000000000 ) ) ;
#17929 = ADVANCED_FACE ( 'NONE', ( #4539 ), #13750, .F. ) ;
#17930 = B_SPLINE_CURVE_WITH_KNOTS ( 'NONE', 3,
 ( #16729, #18128, #9, #10525, #15123, #9122 ),
 .UNSPECIFIED., .F., .F.,
 ( 4, 2, 4 ),
 ( 4.462636695653044375E-07, 0.001879885036799765685, 0.003759323809929966155 ),
 .UNSPECIFIED. ) ;
#17931 = VERTEX_POINT ( 'NONE', #6223 ) ;
#17932 = EDGE_CURVE ( 'NONE', #18641, #5854, #15377, .T. ) ;
#17933 = AXIS2_PLACEMENT_3D ( 'NONE', #9452, #14342, #14042 ) ;
#17934 = CYLINDRICAL_SURFACE ( 'NONE', #1016, 5.700000000000001954 ) ;
#17935 = CARTESIAN_POINT ( 'NONE',  ( 5.699999999999994849, -0.9027913098498965283, -7.812499995903224637 ) ) ;
#17936 = VERTEX_POINT ( 'NONE', #16858 ) ;
#17937 = DIRECTION ( 'NONE',  ( -0.9773501006361904331, 0.000000000000000000, 0.2116288751244229938 ) ) ;
#17938 = EDGE_CURVE ( 'NONE', #1421, #2524, #16661, .T. ) ;
#17939 = CARTESIAN_POINT ( 'NONE',  ( 6.843749997951615427, 4.233219804643887585, -2.444050593749990785 ) ) ;
#17940 = FACE_BOUND ( 'NONE', #8262, .T. ) ;
#17941 = ORIENTED_EDGE ( 'NONE', *, *, #4373, .T. ) ;
#17942 = CARTESIAN_POINT ( 'NONE',  ( -7.626241948324210540, -16.73597674598852336, -35.00000000000000000 ) ) ;
#17943 = VERTEX_POINT ( 'NONE', #10848 ) ;
#17944 = CARTESIAN_POINT ( 'NONE',  ( 2.255998204157473097, -17.85806462366060288, -35.00000000000000000 ) ) ;
#17945 = ORIENTED_EDGE ( 'NONE', *, *, #9588, .F. ) ;
#17946 = FILL_AREA_STYLE ('',( #5723 ) ) ;
#17947 = FACE_OUTER_BOUND ( 'NONE', #18395, .T. ) ;
#17948 = DIRECTION ( 'NONE',  ( 1.000000000000000000, 0.000000000000000000, 0.000000000000000000 ) ) ;
#17949 = LINE ( 'NONE', #4241, #16172 ) ;
#17950 = VECTOR ( 'NONE', #19229, 1000.000000000000000 ) ;
#17951 = VECTOR ( 'NONE', #12098, 1000.000000000000000 ) ;
#17952 = CARTESIAN_POINT ( 'NONE',  ( -11.00000000000000355, 4.215373648918918192, 3.375000000000000888 ) ) ;
#17953 = ORIENTED_EDGE ( 'NONE', *, *, #11951, .F. ) ;
#17954 = AXIS2_PLACEMENT_3D ( 'NONE', #12958, #8548, #6833 ) ;
#17955 = EDGE_CURVE ( 'NONE', #15001, #5363, #11753, .T. ) ;
#17956 = CYLINDRICAL_SURFACE ( 'NONE', #8789, 4.000000000000000000 ) ;
#17957 = B_SPLINE_CURVE_WITH_KNOTS ( 'NONE', 3,
 ( #8994, #7367, #14804, #994 ),
 .UNSPECIFIED., .F., .F.,
 ( 4, 4 ),
 ( 2.324263106244728226E-07, 0.0006888201370294799210 ),
 .UNSPECIFIED. ) ;
#17958 = ORIENTED_EDGE ( 'NONE', *, *, #3671, .T. ) ;
#17959 = B_SPLINE_CURVE_WITH_KNOTS ( 'NONE', 3,
 ( #3751, #18856, #9874, #14158 ),
 .UNSPECIFIED., .F., .F.,
 ( 4, 4 ),
 ( 0.005258214619651938905, 0.005948481662034165590 ),
 .UNSPECIFIED. ) ;
#17960 = DIRECTION ( 'NONE',  ( -7.654042494670959086E-17, 0.6250000000000002220, -0.7806247497997996776 ) ) ;
#17961 = CIRCLE ( 'NONE', #10937, 4.400000000000001243 ) ;
#17962 = FACE_OUTER_BOUND ( 'NONE', #18854, .T. ) ;
#17963 = AXIS2_PLACEMENT_3D ( 'NONE', #877, #19077, #14285 ) ;
#17964 = CARTESIAN_POINT ( 'NONE',  ( -8.671566133830875600, 15.77352024078954429, -32.00000000000000000 ) ) ;
#17965 = CONICAL_SURFACE ( 'NONE', #8367, 9.000000000000001776, 0.6898000447336081198 ) ;
#17966 = DIRECTION ( 'NONE',  ( 1.000000000000000000, 0.000000000000000000, 0.000000000000000000 ) ) ;
#17967 = VERTEX_POINT ( 'NONE', #7734 ) ;
#17968 = CARTESIAN_POINT ( 'NONE',  ( 11.96874999795161365, -1.773574444220693325, -4.620319390059842490 ) ) ;
#17969 = ORIENTED_EDGE ( 'NONE', *, *, #15579, .T. ) ;
#17970 = CARTESIAN_POINT ( 'NONE',  ( -3.270778111535363131, -3.632567103900500971, -10.46874999795161720 ) ) ;
#17971 = PRESENTATION_STYLE_ASSIGNMENT (( #3883 ) ) ;
#17972 = CIRCLE ( 'NONE', #19228, 0.9999999999999974465 ) ;
#17973 = EDGE_LOOP ( 'NONE', ( #10146, #2032, #10309, #17576, #18403, #16223 ) ) ;
#17974 = EDGE_CURVE ( 'NONE', #8529, #5313, #7364, .T. ) ;
#17975 = EDGE_LOOP ( 'NONE', ( #7355, #458, #13568, #11161 ) ) ;
#17976 = DIRECTION ( 'NONE',  ( -1.000000000000000000, -0.000000000000000000, -0.000000000000000000 ) ) ;
#17977 = CARTESIAN_POINT ( 'NONE',  ( 11.46874999795161543, -2.444050593750019651, 4.233219804643871598 ) ) ;
#17978 = ORIENTED_EDGE ( 'NONE', *, *, #2710, .T. ) ;
#17979 = VECTOR ( 'NONE', #1176, 1000.000000000000000 ) ;
#17980 = CARTESIAN_POINT ( 'NONE',  ( 5.575441324182695446, 1.185096637661215757, -12.00000000000000533 ) ) ;
#17981 = MECHANICAL_DESIGN_GEOMETRIC_PRESENTATION_REPRESENTATION (  '', ( #2320 ), #11902 ) ;
#17982 = ORIENTED_EDGE ( 'NONE', *, *, #11282, .T. ) ;
#17983 = EDGE_CURVE ( 'NONE', #4324, #9831, #17707, .T. ) ;
#17984 = LINE ( 'NONE', #10479, #10625 ) ;
#17985 = AXIS2_PLACEMENT_3D ( 'NONE', #14410, #2098, #17602 ) ;
#17986 = EDGE_LOOP ( 'NONE', ( #19452, #13921, #15085, #16765 ) ) ;
#17987 = DIRECTION ( 'NONE',  ( 0.000000000000000000, 0.000000000000000000, 1.000000000000000000 ) ) ;
#17988 = CARTESIAN_POINT ( 'NONE',  ( -6.626241948324210540, -16.73597674598852336, -35.00000000000000000 ) ) ;
#17989 = CARTESIAN_POINT ( 'NONE',  ( 7.343749997951615427, 0.7741991708318887166, -4.888101187500000222 ) ) ;
#17990 = CARTESIAN_POINT ( 'NONE',  ( 2.789999999999999147, 0.000000000000000000, 0.000000000000000000 ) ) ;
#17991 = CIRCLE ( 'NONE', #8411, 8.000000000000000000 ) ;
#17992 = CARTESIAN_POINT ( 'NONE',  ( 2.789679245949058917, 20.70663861606308487, -12.51925356660738053 ) ) ;
#17993 = FILL_AREA_STYLE_COLOUR ( '', #18347 ) ;
#17994 = DIRECTION ( 'NONE',  ( -1.000000000000000000, 0.000000000000000000, 0.000000000000000000 ) ) ;
#17995 = ORIENTED_EDGE ( 'NONE', *, *, #9921, .T. ) ;
#17996 = EDGE_CURVE ( 'NONE', #12398, #2239, #14099, .T. ) ;
#17997 = PRODUCT_RELATED_PRODUCT_CATEGORY ( 'part', '', ( #12896 ) ) ;
#17998 = DIRECTION ( 'NONE',  ( -1.000000000000000000, -0.000000000000000000, -0.000000000000000000 ) ) ;
#17999 = FACE_BOUND ( 'NONE', #18762, .T. ) ;
#18000 = CLOSED_SHELL ( 'NONE', ( #1621, #8556, #3209, #3200, #14242, #9187 ) ) ;
#18001 = B_SPLINE_CURVE_WITH_KNOTS ( 'NONE', 3,
 ( #19298, #2585, #9928, #14619, #11323, #17422 ),
 .UNSPECIFIED., .F., .F.,
 ( 4, 2, 4 ),
 ( 4.462636678151279571E-07, 0.001879885020955181143, 0.003759323778242547407 ),
 .UNSPECIFIED. ) ;
#18002 = UNCERTAINTY_MEASURE_WITH_UNIT (LENGTH_MEASURE( 1.000000000000000082E-05 ), #11074, 'distance_accuracy_value', 'NONE');
#18003 = CARTESIAN_POINT ( 'NONE',  ( 6.234374998975811266, 4.584782303107598267, -2.647025296874989664 ) ) ;
#18004 = CARTESIAN_POINT ( 'NONE',  ( -2.850000000000058265, -4.936344801571268093, -7.312499995903225525 ) ) ;
#18005 = ORIENTED_EDGE ( 'NONE', *, *, #17251, .F. ) ;
#18006 = EDGE_CURVE ( 'NONE', #7032, #11518, #550, .T. ) ;
#18007 = DIRECTION ( 'NONE',  ( -1.000000000000000000, -0.000000000000000000, 0.000000000000000000 ) ) ;
#18008 = EDGE_CURVE ( 'NONE', #12785, #2162, #16977, .T. ) ;
#18009 = CARTESIAN_POINT ( 'NONE',  ( 2.789999999999999147, 24.34211360614310848, -7.909232158574561744 ) ) ;
#18010 = APPLICATION_CONTEXT ( 'automotive_design' ) ;
#18011 = ORIENTED_EDGE ( 'NONE', *, *, #15378, .T. ) ;
#18012 = CARTESIAN_POINT ( 'NONE',  ( 7.843749997951614539, 3.270778111535313837, 3.632567103900546712 ) ) ;
#18013 = DIRECTION ( 'NONE',  ( -1.000000000000000000, -0.000000000000000000, -0.000000000000000000 ) ) ;
#18014 = VECTOR ( 'NONE', #6989, 1000.000000000000000 ) ;
#18015 = CARTESIAN_POINT ( 'NONE',  ( 12.46874999795161543, 3.632567103900569361, -3.270778111535288080 ) ) ;
#18016 = CARTESIAN_POINT ( 'NONE',  ( 1.749999999999998002, 0.000000000000000000, 0.000000000000000000 ) ) ;
#18017 = EDGE_CURVE ( 'NONE', #14278, #16953, #6733, .T. ) ;
#18018 = ORIENTED_EDGE ( 'NONE', *, *, #385, .T. ) ;
#18019 = LINE ( 'NONE', #2791, #15547 ) ;
#18020 =( LENGTH_UNIT ( ) NAMED_UNIT ( * ) SI_UNIT ( .MILLI., .METRE. ) );
#18021 = CARTESIAN_POINT ( 'NONE',  ( 2.500000000000002220, 0.000000000000000000, 0.000000000000000000 ) ) ;
#18022 = CARTESIAN_POINT ( 'NONE',  ( 6.000000000000005329, -3.980288726281172656E-14, 5.700000000000001066 ) ) ;
#18023 = VERTEX_POINT ( 'NONE', #3342 ) ;
#18024 = CARTESIAN_POINT ( 'NONE',  ( 1.749999999999998002, 24.89775460606832524, 12.96210679857795256 ) ) ;
#18025 = ORIENTED_EDGE ( 'NONE', *, *, #4691, .F. ) ;
#18027 = ADVANCED_FACE ( 'NONE', ( #1933 ), #15846, .T. ) ;
#18026 = EDGE_CURVE ( 'NONE', #15829, #11710, #8337, .T. ) ;
#18028 = CARTESIAN_POINT ( 'NONE',  ( 6.000000000000005329, 0.000000000000000000, 4.400000000000000355 ) ) ;
#18029 = CARTESIAN_POINT ( 'NONE',  ( 11.46874999795161543, 4.888101187500000222, -2.993098736590125853E-16 ) ) ;
#18030 = FACE_OUTER_BOUND ( 'NONE', #16846, .T. ) ;
#18031 = DIRECTION ( 'NONE',  ( -1.000000000000000000, 0.000000000000000000, 0.000000000000000000 ) ) ;
#18032 = CLOSED_SHELL ( 'NONE', ( #3130, #4803, #18339, #6543, #1150, #16648, #11766, #14714, #8031, #10640, #10211, #16755, #2801, #5079, #11056, #3735, #1351, #16790, #16147, #10572, #3950, #2984, #9571, #15733, #8325, #8403, #10161, #13811, #17546, #9597, #8727, #10449, #10505, #6050, #7473, #13993, #4671, #10795, #19144, #16036, #3060, #18919, #15127, #8232, #6922, #4193, #3318 ) ) ;
#18033 = ORIENTED_EDGE ( 'NONE', *, *, #12551, .T. ) ;
#18034 = AXIS2_PLACEMENT_3D ( 'NONE', #3878, #5283, #17688 ) ;
#18035 = DIRECTION ( 'NONE',  ( -1.000000000000000000, 0.000000000000000000, 0.000000000000000000 ) ) ;
#18036 = DIRECTION ( 'NONE',  ( 0.000000000000000000, 0.000000000000000000, -1.000000000000000000 ) ) ;
#18037 = EDGE_LOOP ( 'NONE', ( #4308, #11759, #6376, #4737, #11659, #18955, #8471, #17256 ) ) ;
#18038 = B_SPLINE_CURVE_WITH_KNOTS ( 'NONE', 3,
 ( #15380, #9179, #8243, #12848, #9379, #15479, #5336, #18847, #2039, #1669 ),
 .UNSPECIFIED., .F., .F.,
 ( 4, 3, 3, 4 ),
 ( 0.000000000000000000, 0.0001875345074742635362, 0.0003808595644229699441, 0.0005744879655065563686 ),
 .UNSPECIFIED. ) ;
#18039 = AXIS2_PLACEMENT_3D ( 'NONE', #5260, #865, #2543 ) ;
#18040 = DIRECTION ( 'NONE',  ( 0.000000000000000000, 0.000000000000000000, 1.000000000000000000 ) ) ;
#18041 = ORIENTED_EDGE ( 'NONE', *, *, #6817, .F. ) ;
#18042 = CARTESIAN_POINT ( 'NONE',  ( 3.270778111535338262, 3.632567103900523620, -10.84374999795161543 ) ) ;
#18043 = CARTESIAN_POINT ( 'NONE',  ( 8.776855558857221240, 3.635492607468361559, 12.00000000000000000 ) ) ;
#18044 = CARTESIAN_POINT ( 'NONE',  ( 11.46874999795161543, 4.888101187500000222, -2.993098736590125853E-16 ) ) ;
#18045 = ORIENTED_EDGE ( 'NONE', *, *, #12251, .T. ) ;
#18046 = CARTESIAN_POINT ( 'NONE',  ( 2.789999999999999147, -24.15498966839966855, 5.391175441198523544 ) ) ;
#18047 = ORIENTED_EDGE ( 'NONE', *, *, #285, .F. ) ;
#18048 = CARTESIAN_POINT ( 'NONE',  ( 2.718184757033982990, 18.89296398180191616, 16.91181672897740640 ) ) ;
#18049 = ORIENTED_EDGE ( 'NONE', *, *, #7786, .F. ) ;
#18050 = DIRECTION ( 'NONE',  ( 0.000000000000000000, 0.000000000000000000, 1.000000000000000000 ) ) ;
#18051 = DIRECTION ( 'NONE',  ( 0.8660254037844398178, -6.047423072554923456E-15, 0.4999999999999979461 ) ) ;
#18052 = CARTESIAN_POINT ( 'NONE',  ( -2.246813503491864150, -4.409619785863891472, -12.96874999795161543 ) ) ;
#18053 = DIRECTION ( 'NONE',  ( 1.000000000000000000, -0.000000000000000000, -0.000000000000000000 ) ) ;
#18054 = AXIS2_PLACEMENT_3D ( 'NONE', #5492, #14316, #13209 ) ;
#18055 = CARTESIAN_POINT ( 'NONE',  ( 13.00000000000000178, 0.7156116249825889009, 4.835865888676774915 ) ) ;
#18056 = ORIENTED_EDGE ( 'NONE', *, *, #9215, .F. ) ;
#18057 = DIRECTION ( 'NONE',  ( 1.000000000000000000, 0.000000000000000000, 0.000000000000000000 ) ) ;
#18058 = ORIENTED_EDGE ( 'NONE', *, *, #14554, .T. ) ;
#18059 = CARTESIAN_POINT ( 'NONE',  ( 7.500000000000005329, 2.620002426024544029, -5.142044285764751699 ) ) ;
#18060 = DIRECTION ( 'NONE',  ( -0.000000000000000000, -0.000000000000000000, 1.000000000000000000 ) ) ;
#18061 = CIRCLE ( 'NONE', #7502, 3.000000000000000000 ) ;
#18062 = DIRECTION ( 'NONE',  ( -1.000000000000000000, -0.000000000000000000, -0.000000000000000000 ) ) ;
#18063 = CARTESIAN_POINT ( 'NONE',  ( 0.5109457054261454800, -4.861323657744410554, -14.46874999795161720 ) ) ;
#18064 = CARTESIAN_POINT ( 'NONE',  ( 13.00000000000000178, 0.000000000000000000, 0.000000000000000000 ) ) ;
#18065 = ORIENTED_EDGE ( 'NONE', *, *, #4518, .F. ) ;
#18066 = CARTESIAN_POINT ( 'NONE',  ( -0.2590123213420971182, 4.942249507334556924, -7.968749997951616315 ) ) ;
#18067 = DIRECTION ( 'NONE',  ( 1.000000000000000000, 0.000000000000000000, 0.000000000000000000 ) ) ;
#18068 = CARTESIAN_POINT ( 'NONE',  ( -4.465502636338010589, 1.988169868018623720, -14.46874999795161720 ) ) ;
#18069 = EDGE_CURVE ( 'NONE', #11964, #9059, #18940, .T. ) ;
#18070 = ORIENTED_EDGE ( 'NONE', *, *, #17138, .F. ) ;
#18071 = ORIENTED_EDGE ( 'NONE', *, *, #5470, .T. ) ;
#18072 = CARTESIAN_POINT ( 'NONE',  ( 4.476417968967386862, 17.43449690031536292, -35.00000000000000000 ) ) ;
#18073 = CARTESIAN_POINT ( 'NONE',  ( 14.46874999795161720, -4.861323657744410554, 0.5109457054261454800 ) ) ;
#18074 = VERTEX_POINT ( 'NONE', #5232 ) ;
#18075 = AXIS2_PLACEMENT_3D ( 'NONE', #6510, #4633, #12638 ) ;
#18076 = CARTESIAN_POINT ( 'NONE',  ( -14.86923836996421144, -11.47363181547641275, -35.00000000000000000 ) ) ;
#18077 = ORIENTED_EDGE ( 'NONE', *, *, #9623, .F. ) ;
#18078 = CIRCLE ( 'NONE', #9458, 5.200000000000000178 ) ;
#18079 = LINE ( 'NONE', #17877, #18912 ) ;
#18080 = CARTESIAN_POINT ( 'NONE',  ( -11.00000000000000355, 4.215373648918918192, 3.375000000000000888 ) ) ;
#18081 = ORIENTED_EDGE ( 'NONE', *, *, #16872, .F. ) ;
#18082 = EDGE_CURVE ( 'NONE', #5861, #6550, #8630, .T. ) ;
#18083 = LINE ( 'NONE', #10580, #17979 ) ;
#18084 = CARTESIAN_POINT ( 'NONE',  ( -6.634287453978999771, 5.335127875949178033, -0.3142460757452209541 ) ) ;
#18085 = DIRECTION ( 'NONE',  ( 1.000000000000000000, 0.000000000000000000, 0.000000000000000000 ) ) ;
#18086 = VECTOR ( 'NONE', #12428, 1000.000000000000000 ) ;
#18087 = ORIENTED_EDGE ( 'NONE', *, *, #4528, .T. ) ;
#18088 = CARTESIAN_POINT ( 'NONE',  ( 2.789895104907798906, 20.67847077765723185, -12.51925356660737876 ) ) ;
#18089 = CYLINDRICAL_SURFACE ( 'NONE', #9671, 1.000000000000004441 ) ;
#18090 = EDGE_CURVE ( 'NONE', #12547, #17754, #642, .T. ) ;
#18091 = VECTOR ( 'NONE', #409, 1000.000000000000000 ) ;
#18092 = VERTEX_POINT ( 'NONE', #18740 ) ;
#18093 = DIRECTION ( 'NONE',  ( 1.000000000000000000, 0.000000000000000000, 0.000000000000000000 ) ) ;
#18094 = CARTESIAN_POINT ( 'NONE',  ( 1.394999999999999574, 4.633866840649313090, -27.68468304288253989 ) ) ;
#18095 = CARTESIAN_POINT ( 'NONE',  ( -41.99999999999999289, -2.000000000000001776, -2.000000000000000000 ) ) ;
#18096 = CARTESIAN_POINT ( 'NONE',  ( 4.861323657744411442, 0.5109457054261445919, -9.468749997951615427 ) ) ;
#18097 = CARTESIAN_POINT ( 'NONE',  ( -5.668774803599165857, -0.5958122406255588199, -10.31249999590322552 ) ) ;
#18098 = EDGE_LOOP ( 'NONE', ( #13852, #9990, #14062, #18576 ) ) ;
#18099 = CARTESIAN_POINT ( 'NONE',  ( -20.63749999999999574, 0.000000000000000000, 0.000000000000000000 ) ) ;
#18100 = DIRECTION ( 'NONE',  ( 0.000000000000000000, 0.000000000000000000, 1.000000000000000000 ) ) ;
#18101 = AXIS2_PLACEMENT_3D ( 'NONE', #12897, #12996, #3880 ) ;
#18102 = VERTEX_POINT ( 'NONE', #3534 ) ;
#18103 = FACE_OUTER_BOUND ( 'NONE', #16065, .T. ) ;
#18104 = CIRCLE ( 'NONE', #9169, 2.524999999999996803 ) ;
#18105 = ADVANCED_FACE ( 'NONE', ( #7930 ), #6717, .F. ) ;
#18106 = CARTESIAN_POINT ( 'NONE',  ( 7.343749997951615427, -4.620319390059841602, 1.773574444220693103 ) ) ;
#18107 = EDGE_CURVE ( 'NONE', #14054, #6506, #13772, .T. ) ;
#18108 = CARTESIAN_POINT ( 'NONE',  ( -5.000000000000000000, 1.999999999999998668, 37.99999999999999289 ) ) ;
#18109 = DIRECTION ( 'NONE',  ( -1.000000000000000000, 0.000000000000000000, -0.000000000000000000 ) ) ;
#18110 = ADVANCED_FACE ( 'NONE', ( #17242 ), #15703, .T. ) ;
#18111 = ORIENTED_EDGE ( 'NONE', *, *, #6150, .F. ) ;
#18112 = LINE ( 'NONE', #5788, #11405 ) ;
#18113 = CARTESIAN_POINT ( 'NONE',  ( -5.000000000000000000, 0.000000000000000000, 41.99999999999999289 ) ) ;
#18114 = CARTESIAN_POINT ( 'NONE',  ( 7.000000000000005329, -1.761396867937238486, 5.421022142882364392 ) ) ;
#18115 = ORIENTED_EDGE ( 'NONE', *, *, #1710, .F. ) ;
#18116 = EDGE_CURVE ( 'NONE', #11695, #16740, #12506, .T. ) ;
#18117 = FACE_BOUND ( 'NONE', #8948, .T. ) ;
#18118 = VECTOR ( 'NONE', #2868, 1000.000000000000000 ) ;
#18119 = EDGE_LOOP ( 'NONE', ( #820, #614, #19247 ) ) ;
#18120 = CARTESIAN_POINT ( 'NONE',  ( 0.000000000000000000, 0.000000000000000000, 0.000000000000000000 ) ) ;
#18121 = CIRCLE ( 'NONE', #13323, 6.000000000000020428 ) ;
#18122 = DIRECTION ( 'NONE',  ( 0.000000000000000000, 0.000000000000000000, 1.000000000000000000 ) ) ;
#18123 = DIRECTION ( 'NONE',  ( 0.000000000000000000, 0.000000000000000000, -1.000000000000000000 ) ) ;
#18124 = CARTESIAN_POINT ( 'NONE',  ( 4.780397808154257078, -1.280903732194453637, -14.34374999795161543 ) ) ;
#18125 = ORIENTED_EDGE ( 'NONE', *, *, #10432, .T. ) ;
#18126 = CARTESIAN_POINT ( 'NONE',  ( -1.001543065824775120E-15, -9.165435523385328409, -6.527800000000000047 ) ) ;
#18127 = ADVANCED_FACE ( 'NONE', ( #15947 ), #12946, .F. ) ;
#18128 = CARTESIAN_POINT ( 'NONE',  ( 2.030753603471114221, 24.32906614999634698, -12.98165646470055634 ) ) ;
#18129 = ORIENTED_EDGE ( 'NONE', *, *, #9622, .F. ) ;
#18130 = CIRCLE ( 'NONE', #16865, 0.9999999999999974465 ) ;
#18131 = EDGE_CURVE ( 'NONE', #12048, #344, #13150, .T. ) ;
#18132 = AXIS2_PLACEMENT_3D ( 'NONE', #7125, #2349, #13342 ) ;
#18133 = CARTESIAN_POINT ( 'NONE',  ( 3.954556930911861112, 2.873153789725825913, -14.84374999795161543 ) ) ;
#18134 = CARTESIAN_POINT ( 'NONE',  ( 1.510506337161829027, -4.648860486681964055, -10.84374999795161543 ) ) ;
#18135 = VERTEX_POINT ( 'NONE', #444 ) ;
#18136 = LINE ( 'NONE', #16538, #5910 ) ;
#18137 = CARTESIAN_POINT ( 'NONE',  ( 1.749999999999998002, 19.67366047555558950, -20.02152543075324687 ) ) ;
#18138 = DIRECTION ( 'NONE',  ( -1.000000000000000000, -4.060088635510494296E-15, 0.000000000000000000 ) ) ;
#18139 = ORIENTED_EDGE ( 'NONE', *, *, #3353, .F. ) ;
#18140 = LINE ( 'NONE', #1229, #15666 ) ;
#18141 = ORIENTED_EDGE ( 'NONE', *, *, #12803, .T. ) ;
#18142 = FACE_OUTER_BOUND ( 'NONE', #17070, .T. ) ;
#18143 = ORIENTED_EDGE ( 'NONE', *, *, #14122, .F. ) ;
#18144 = CARTESIAN_POINT ( 'NONE',  ( 0.07181523211953112773, 23.19431517146946931, -10.24584646439514657 ) ) ;
#18145 = FACE_OUTER_BOUND ( 'NONE', #14007, .T. ) ;
#18146 = FACE_OUTER_BOUND ( 'NONE', #16467, .T. ) ;
#18147 = CARTESIAN_POINT ( 'NONE',  ( 6.968749997951614539, -4.620319390059841602, 1.773574444220693103 ) ) ;
#18148 = AXIS2_PLACEMENT_3D ( 'NONE', #2872, #8986, #11688 ) ;
#18149 = DIRECTION ( 'NONE',  ( 1.000000000000000000, 0.000000000000000000, 0.000000000000000000 ) ) ;
#18150 = CIRCLE ( 'NONE', #13989, 6.735000000000022524 ) ;
#18151 = EDGE_CURVE ( 'NONE', #3605, #14863, #6740, .T. ) ;
#18152 = ORIENTED_EDGE ( 'NONE', *, *, #134, .F. ) ;
#18153 = DIRECTION ( 'NONE',  ( 0.000000000000000000, 0.000000000000000000, -1.000000000000000000 ) ) ;
#18154 = DIRECTION ( 'NONE',  ( -1.000000000000000000, -0.000000000000000000, -0.000000000000000000 ) ) ;
#18155 =( BOUNDED_SURFACE ( )  B_SPLINE_SURFACE ( 1, 2, ( 
 ( #3645, #8348, #15761, #12855, #653, #3843, #12756, #5137, #11253, #17357, #6727, #18952, #9768, #2243, #15217, #13807, #6191 ),
 ( #17844, #4138, #10251, #1139, #18409, #11740, #7492, #18314, #15316, #19708, #104, #1037, #16917, #4703, #203, #13611, #9114 ) ),
 .UNSPECIFIED., .F., .F., .F. ) 
 B_SPLINE_SURFACE_WITH_KNOTS ( ( 2, 2 ),
 ( 3, 2, 2, 2, 2, 2, 2, 2, 3 ),
 ( 0.000000000000000000, 1.000000000000000000 ),
 ( 0.000000000000000000, 0.05000000000000000278, 0.1000000000000000056, 0.1499999999999999944, 0.2000000000000000111, 0.2500000000000000000, 0.2999999999999999889, 0.3499999999999999778, 0.4000000000000000222 ),
 .UNSPECIFIED. ) 
 GEOMETRIC_REPRESENTATION_ITEM ( )  RATIONAL_B_SPLINE_SURFACE ( (
 ( 1.000000000000000000, 0.9876883405951377704, 1.000000000000000000, 0.9876883405951377704, 1.000000000000000000, 0.9876883405951377704, 1.000000000000000000, 0.9876883405951377704, 1.000000000000000000, 0.9876883405951377704, 1.000000000000000000, 0.9876883405951377704, 1.000000000000000000, 0.9876883405951377704, 1.000000000000000000, 0.9876883405951377704, 1.000000000000000000),
 ( 1.000000000000000000, 0.9876883405951377704, 1.000000000000000000, 0.9876883405951377704, 1.000000000000000000, 0.9876883405951377704, 1.000000000000000000, 0.9876883405951377704, 1.000000000000000000, 0.9876883405951377704, 1.000000000000000000, 0.9876883405951377704, 1.000000000000000000, 0.9876883405951377704, 1.000000000000000000, 0.9876883405951377704, 1.000000000000000000) ) ) 
 REPRESENTATION_ITEM ( '' )  SURFACE ( )  );
#18156 = EDGE_CURVE ( 'NONE', #4917, #5485, #16993, .T. ) ;
#18157 = ORIENTED_EDGE ( 'NONE', *, *, #12794, .T. ) ;
#18158 = EDGE_CURVE ( 'NONE', #9320, #18721, #9659, .T. ) ;
#18159 = CARTESIAN_POINT ( 'NONE',  ( 0.5321745087963413168, -24.44564404695853455, 11.58891744060097295 ) ) ;
#18160 = CARTESIAN_POINT ( 'NONE',  ( 2.789999999999999147, -16.37294372382844543, -18.55949924794910544 ) ) ;
#18161 = VECTOR ( 'NONE', #11280, 1000.000000000000000 ) ;
#18162 = ORIENTED_EDGE ( 'NONE', *, *, #13955, .F. ) ;
#18163 = CYLINDRICAL_SURFACE ( 'NONE', #350, 0.9999999999999974465 ) ;
#18164 = CARTESIAN_POINT ( 'NONE',  ( 8.000000000000000000, 0.000000000000000000, 0.000000000000000000 ) ) ;
#18165 = CIRCLE ( 'NONE', #9543, 7.800000000000000711 ) ;
#18166 = CARTESIAN_POINT ( 'NONE',  ( 0.000000000000000000, 0.000000000000000000, 0.000000000000000000 ) ) ;
#18167 = ORIENTED_EDGE ( 'NONE', *, *, #14108, .T. ) ;
#18168 = CARTESIAN_POINT ( 'NONE',  ( 4.861323657744406113, -0.5109457054261780096, -13.46874999795161543 ) ) ;
#18169 = DIRECTION ( 'NONE',  ( 1.000000000000000000, 0.000000000000000000, 0.000000000000000000 ) ) ;
#18170 = CARTESIAN_POINT ( 'NONE',  ( 5.574407415329156734, -1.493657965219523209, -13.50000000000000533 ) ) ;
#18171 = CARTESIAN_POINT ( 'NONE',  ( 0.000000000000000000, 0.000000000000000000, 0.000000000000000000 ) ) ;
#18172 = ORIENTED_EDGE ( 'NONE', *, *, #11494, .T. ) ;
#18173 = ORIENTED_EDGE ( 'NONE', *, *, #16910, .T. ) ;
#18174 = DIRECTION ( 'NONE',  ( -1.000000000000000000, 0.000000000000000000, 0.000000000000000000 ) ) ;
#18175 = CARTESIAN_POINT ( 'NONE',  ( 0.5958122406256377568, 5.668774803599156975, -9.312499995903225525 ) ) ;
#18176 = EDGE_LOOP ( 'NONE', ( #15954, #9268, #2434, #18087 ) ) ;
#18177 = ADVANCED_FACE ( 'NONE', ( #10237, #2329 ), #5708, .T. ) ;
#18178 = CIRCLE ( 'NONE', #907, 1.000000000000002665 ) ;
#18179 = CARTESIAN_POINT ( 'NONE',  ( 0.02436607992776108206, -24.15498966839966855, 5.391175441198523544 ) ) ;
#18180 = ORIENTED_EDGE ( 'NONE', *, *, #13955, .T. ) ;
#18181 = CARTESIAN_POINT ( 'NONE',  ( 2.849999999999954348, -4.936344801571327601, -6.000000000000005329 ) ) ;
#18182 = EDGE_LOOP ( 'NONE', ( #10536, #5608, #4513, #8871, #3978, #3383, #4159, #5611 ) ) ;
#18183 = AXIS2_PLACEMENT_3D ( 'NONE', #4455, #16663, #18264 ) ;
#18184 = ADVANCED_FACE ( 'NONE', ( #8827 ), #17934, .T. ) ;
#18185 = DIRECTION ( 'NONE',  ( 0.000000000000000000, 0.000000000000000000, 1.000000000000000000 ) ) ;
#18186 = CARTESIAN_POINT ( 'NONE',  ( 0.000000000000000000, 15.74360496233409634, -18.28042085475261302 ) ) ;
#18187 = CARTESIAN_POINT ( 'NONE',  ( -1.255998204157475318, -17.85806462366060288, 32.00000000000000000 ) ) ;
#18188 = CIRCLE ( 'NONE', #613, 1.000000000000000888 ) ;
#18189 = ORIENTED_EDGE ( 'NONE', *, *, #12127, .T. ) ;
#18190 = EDGE_CURVE ( 'NONE', #15562, #11187, #5148, .T. ) ;
#18191 = CYLINDRICAL_SURFACE ( 'NONE', #14596, 28.06981291497571362 ) ;
#18192 = CARTESIAN_POINT ( 'NONE',  ( 0.8956445960621760571, 24.59653223688280121, 12.96989951879416125 ) ) ;
#18193 = VERTEX_POINT ( 'NONE', #3930 ) ;
#18194 = CYLINDRICAL_SURFACE ( 'NONE', #18148, 1.000000000000000888 ) ;
#18195 = LINE ( 'NONE', #9091, #2452 ) ;
#18196 = PRODUCT_DEFINITION_CONTEXT ( 'detailed design', #2280, 'design' ) ;
#18197 = DIRECTION ( 'NONE',  ( 1.000000000000000000, 0.000000000000000000, 0.000000000000000000 ) ) ;
#18198 = CARTESIAN_POINT ( 'NONE',  ( 2.351340098004231383, 23.41653927703715965, 12.93238701107315514 ) ) ;
#18199 = CARTESIAN_POINT ( 'NONE',  ( -15.00000000000000355, 3.434748899119118626, 2.750000000000001332 ) ) ;
#18200 = VERTEX_POINT ( 'NONE', #17831 ) ;
#18201 = FACE_OUTER_BOUND ( 'NONE', #12455, .T. ) ;
#18202 = DIRECTION ( 'NONE',  ( 0.000000000000000000, 0.3090169943749350723, 0.9510565162951576390 ) ) ;
#18203 = ORIENTED_EDGE ( 'NONE', *, *, #3337, .T. ) ;
#18204 = CARTESIAN_POINT ( 'NONE',  ( 8.968749997951611874, -1.280903732194386579, -4.780397808154273953 ) ) ;
#18205 = EDGE_CURVE ( 'NONE', #8877, #10068, #16331, .T. ) ;
#18206 = B_SPLINE_CURVE_WITH_KNOTS ( 'NONE', 3,
 ( #9985, #15146, #18250, #16456 ),
 .UNSPECIFIED., .F., .F.,
 ( 4, 4 ),
 ( 0.000000000000000000, 0.001125480700308659687 ),
 .UNSPECIFIED. ) ;
#18207 = FACE_OUTER_BOUND ( 'NONE', #1270, .T. ) ;
#18208 = AXIS2_PLACEMENT_3D ( 'NONE', #4749, #5138, #12458 ) ;
#18209 = CARTESIAN_POINT ( 'NONE',  ( -5.000000000000000000, -2.000000000000001332, 37.99999999999999289 ) ) ;
#18210 = CARTESIAN_POINT ( 'NONE',  ( 6.000000000000005329, 4.936344801571308061, -2.849999999999988987 ) ) ;
#18211 = SHAPE_REPRESENTATION ( 'BR-591', ( #7297, #930, #13066, #296, #15623, #1250, #19450, #18183, #8923, #7942, #616, #3161, #12111, #4438, #10840, #6975, #14355, #6345, #2203 ), #18814 ) ;
#18212 = ORIENTED_EDGE ( 'NONE', *, *, #7522, .F. ) ;
#18213 = CARTESIAN_POINT ( 'NONE',  ( 2.783068945535915439, 24.42321038836782776, -2.248820353273055517 ) ) ;
#18214 = CARTESIAN_POINT ( 'NONE',  ( 13.86923836996420789, -11.47363181547641453, -32.00000000000000000 ) ) ;
#18215 = CARTESIAN_POINT ( 'NONE',  ( -7.940452095251188120E-14, -18.34439787333518268, 15.96555658743757000 ) ) ;
#18216 = ORIENTED_EDGE ( 'NONE', *, *, #19424, .F. ) ;
#18217 = CYLINDRICAL_SURFACE ( 'NONE', #12392, 0.9999999999999974465 ) ;
#18218 = FACE_OUTER_BOUND ( 'NONE', #7131, .T. ) ;
#18219 = CARTESIAN_POINT ( 'NONE',  ( 2.789999999999999147, 18.28042085475301093, -15.74360496233361673 ) ) ;
#18220 = EDGE_CURVE ( 'NONE', #17227, #16305, #10605, .T. ) ;
#18221 = LINE ( 'NONE', #16826, #223 ) ;
#18222 = EDGE_CURVE ( 'NONE', #11827, #7344, #19532, .T. ) ;
#18223 = EDGE_CURVE ( 'NONE', #12464, #8660, #11967, .T. ) ;
#18224 = CYLINDRICAL_SURFACE ( 'NONE', #17637, 3.000000000000000000 ) ;
#18225 = AXIS2_PLACEMENT_3D ( 'NONE', #19412, #19507, #4407 ) ;
#18226 = CARTESIAN_POINT ( 'NONE',  ( 2.783069004973551142, 5.408431875071779693, -23.92277630352788975 ) ) ;
#18227 = ORIENTED_EDGE ( 'NONE', *, *, #19044, .T. ) ;
#18228 = DIRECTION ( 'NONE',  ( 0.000000000000000000, 0.000000000000000000, 1.000000000000000000 ) ) ;
#18229 = CARTESIAN_POINT ( 'NONE',  ( -10.00000000000000000, 0.000000000000000000, 0.000000000000000000 ) ) ;
#18230 = ORIENTED_EDGE ( 'NONE', *, *, #399, .F. ) ;
#18231 = EDGE_CURVE ( 'NONE', #3344, #11304, #18897, .T. ) ;
#18232 = EDGE_CURVE ( 'NONE', #677, #16827, #2609, .T. ) ;
#18233 = CARTESIAN_POINT ( 'NONE',  ( -0.7741991708318890497, 4.888101187500000222, -11.34374999795161543 ) ) ;
#18234 = CARTESIAN_POINT ( 'NONE',  ( 1.039999999999995817, 4.633866840648921404, 27.68468304288260029 ) ) ;
#18235 = VERTEX_POINT ( 'NONE', #2420 ) ;
#18236 = AXIS2_PLACEMENT_3D ( 'NONE', #10299, #13289, #7569 ) ;
#18237 = CARTESIAN_POINT ( 'NONE',  ( 13.31249999590322730, 1.185096637661216201, 5.575441324182695446 ) ) ;
#18238 = AXIS2_PLACEMENT_3D ( 'NONE', #19408, #5790, #1408 ) ;
#18239 = CARTESIAN_POINT ( 'NONE',  ( 12.00000000000000178, 1.469576158976824144E-15, 35.00000000000000000 ) ) ;
#18240 = ORIENTED_EDGE ( 'NONE', *, *, #14888, .T. ) ;
#18241 = CARTESIAN_POINT ( 'NONE',  ( 1.749999999999998002, 4.147968289691286614, 27.76164181293053090 ) ) ;
#18242 = EDGE_LOOP ( 'NONE', ( #6961, #18504, #16911, #11332 ) ) ;
#18243 = DIRECTION ( 'NONE',  ( 0.000000000000000000, 0.000000000000000000, 1.000000000000000000 ) ) ;
#18244 = EDGE_LOOP ( 'NONE', ( #1063, #17145, #8252, #18459 ) ) ;
#18245 = CARTESIAN_POINT ( 'NONE',  ( 1.039999999999996039, 19.67366047555559305, -20.02152543075323976 ) ) ;
#18246 = DIRECTION ( 'NONE',  ( -0.000000000000000000, -0.000000000000000000, 1.000000000000000000 ) ) ;
#18247 = CARTESIAN_POINT ( 'NONE',  ( -1.869200000000000195, 0.000000000000000000, 0.000000000000000000 ) ) ;
#18248 = CARTESIAN_POINT ( 'NONE',  ( 13.00000000000000533, 4.611396867937201272, 3.350375938067096548 ) ) ;
#18249 = ORIENTED_EDGE ( 'NONE', *, *, #14387, .F. ) ;
#18250 = CARTESIAN_POINT ( 'NONE',  ( 12.99999999999998757, -4.496303326521678301, 2.563255015864473130 ) ) ;
#18251 = EDGE_CURVE ( 'NONE', #871, #11866, #13040, .T. ) ;
#18252 = ADVANCED_FACE ( 'NONE', ( #8536 ), #1221, .T. ) ;
#18253 = EDGE_LOOP ( 'NONE', ( #2844, #8019, #19781, #9150, #15701, #6391 ) ) ;
#18254 = CARTESIAN_POINT ( 'NONE',  ( -15.19790265903627180, 9.644882309621941374, -35.00000000000000000 ) ) ;
#18255 = DIRECTION ( 'NONE',  ( 0.000000000000000000, 0.000000000000000000, 1.000000000000000000 ) ) ;
#18256 = ORIENTED_EDGE ( 'NONE', *, *, #16686, .F. ) ;
#18257 = DIRECTION ( 'NONE',  ( 0.000000000000000000, 0.000000000000000000, -1.000000000000000000 ) ) ;
#18258 = CARTESIAN_POINT ( 'NONE',  ( 4.840010801796506890, 3.143139765844590983, -7.500000000000005329 ) ) ;
#18259 = DIRECTION ( 'NONE',  ( 0.000000000000000000, 0.000000000000000000, 1.000000000000000000 ) ) ;
#18260 = EDGE_LOOP ( 'NONE', ( #7606, #18172, #4454, #14157 ) ) ;
#18261 = ADVANCED_FACE ( 'NONE', ( #11444 ), #11631, .T. ) ;
#18262 = CARTESIAN_POINT ( 'NONE',  ( 1.039999999999998259, 12.52377138324223615, 25.12109765559657859 ) ) ;
#18263 = CIRCLE ( 'NONE', #14753, 1.000000000000000888 ) ;
#18264 = DIRECTION ( 'NONE',  ( 1.000000000000000000, 0.000000000000000000, 0.000000000000000000 ) ) ;
#18265 = CONICAL_SURFACE ( 'NONE', #17302, 9.000000000000001776, 0.6898000447336081198 ) ;
#18266 = CARTESIAN_POINT ( 'NONE',  ( 2.718184743034447681, -5.344212458769196594, -24.78695292654926519 ) ) ;
#18267 = CARTESIAN_POINT ( 'NONE',  ( -4.484949146646406426, -3.631840208645763735, -11.81249999590322552 ) ) ;
#18268 = VERTEX_POINT ( 'NONE', #19324 ) ;
#18269 = ORIENTED_EDGE ( 'NONE', *, *, #15075, .F. ) ;
#18270 = CARTESIAN_POINT ( 'NONE',  ( 11.34374999795161543, 4.888101187500000222, -0.7741991708318890497 ) ) ;
#18271 = EDGE_CURVE ( 'NONE', #3690, #2257, #8035, .T. ) ;
#18272 = ORIENTED_EDGE ( 'NONE', *, *, #1855, .T. ) ;
#18273 = DIRECTION ( 'NONE',  ( 1.000000000000000000, 0.000000000000000000, 0.000000000000000000 ) ) ;
#18274 = VERTEX_POINT ( 'NONE', #16043 ) ;
#18275 = FACE_OUTER_BOUND ( 'NONE', #11126, .T. ) ;
#18276 = CIRCLE ( 'NONE', #10285, 4.000000000000000000 ) ;
#18277 = ORIENTED_EDGE ( 'NONE', *, *, #263, .F. ) ;
#18278 = CIRCLE ( 'NONE', #12204, 5.700000000000001954 ) ;
#18279 = CIRCLE ( 'NONE', #2612, 1.000000000000000888 ) ;
#18280 = STYLED_ITEM ( 'NONE', ( #18770 ), #2500 ) ;
#18281 = PLANE ( 'NONE',  #17349 ) ;
#18282 = ADVANCED_FACE ( 'NONE', ( #2516 ), #8624, .T. ) ;
#18283 = CARTESIAN_POINT ( 'NONE',  ( 10.84374999795161543, 4.648860486681953397, -1.510506337161861667 ) ) ;
#18284 = CARTESIAN_POINT ( 'NONE',  ( 0.000000000000000000, 0.000000000000000000, 32.00000000000000000 ) ) ;
#18285 = ORIENTED_EDGE ( 'NONE', *, *, #7739, .F. ) ;
#18286 = DIRECTION ( 'NONE',  ( 0.000000000000000000, 0.000000000000000000, 1.000000000000000000 ) ) ;
#18287 = CARTESIAN_POINT ( 'NONE',  ( 0.8291131470075423504, 24.44424927289185945, 12.96989951879416125 ) ) ;
#18288 = EDGE_LOOP ( 'NONE', ( #18448, #18975, #2459, #18981 ) ) ;
#18289 = CARTESIAN_POINT ( 'NONE',  ( 1.749999999999998002, -12.96210679857767367, -24.89775460606847091 ) ) ;
#18290 = TOROIDAL_SURFACE ( 'NONE', #1034, 24.12539914357697768, 8.000000000000000000 ) ;
#18291 = DIRECTION ( 'NONE',  ( -1.000000000000000000, -0.000000000000000000, -0.000000000000000000 ) ) ;
#18292 = CARTESIAN_POINT ( 'NONE',  ( 0.07181525068722571792, -25.22524549359951962, 2.576941577947320372 ) ) ;
#18293 = VECTOR ( 'NONE', #8793, 1000.000000000000000 ) ;
#18294 = CARTESIAN_POINT ( 'NONE',  ( 5.207209108562820710, -2.318398865532073305, -15.31249999590322552 ) ) ;
#18295 = DIRECTION ( 'NONE',  ( -0.000000000000000000, -0.000000000000000000, -1.000000000000000000 ) ) ;
#18296 = ORIENTED_EDGE ( 'NONE', *, *, #19212, .T. ) ;
#18297 = DIRECTION ( 'NONE',  ( 0.000000000000000000, 0.000000000000000000, 1.000000000000000000 ) ) ;
#18298 = AXIS2_PLACEMENT_3D ( 'NONE', #10780, #15779, #2063 ) ;
#18299 = CARTESIAN_POINT ( 'NONE',  ( -1.800000000000000488, 0.000000000000000000, -4.200000000000000178 ) ) ;
#18300 = EDGE_LOOP ( 'NONE', ( #17778, #16050 ) ) ;
#18301 = DIRECTION ( 'NONE',  ( 0.000000000000000000, 0.000000000000000000, -1.000000000000000000 ) ) ;
#18302 = DIRECTION ( 'NONE',  ( 1.000000000000000000, 0.000000000000000000, 0.000000000000000000 ) ) ;
#18303 = AXIS2_PLACEMENT_3D ( 'NONE', #15672, #4668, #12471 ) ;
#18304 = CIRCLE ( 'NONE', #1370, 4.400000000000000355 ) ;
#18305 = DIRECTION ( 'NONE',  ( 0.000000000000000000, 0.000000000000000000, 1.000000000000000000 ) ) ;
#18306 = LINE ( 'NONE', #16511, #6172 ) ;
#18307 = ORIENTED_EDGE ( 'NONE', *, *, #4044, .F. ) ;
#18308 = AXIS2_PLACEMENT_3D ( 'NONE', #9250, #4642, #13949 ) ;
#18309 = DIRECTION ( 'NONE',  ( -1.000000000000000000, 0.000000000000000000, 0.000000000000000000 ) ) ;
#18310 = FACE_OUTER_BOUND ( 'NONE', #18954, .T. ) ;
#18311 = DIRECTION ( 'NONE',  ( -0.000000000000000000, -0.000000000000000000, 1.000000000000000000 ) ) ;
#18312 = EDGE_LOOP ( 'NONE', ( #14841, #14875, #2036, #8538 ) ) ;
#18313 = DIRECTION ( 'NONE',  ( 1.000000000000000000, 0.000000000000000000, 0.000000000000000000 ) ) ;
#18314 = CARTESIAN_POINT ( 'NONE',  ( 9.968749997951617203, -0.2590123213421313686, 4.942249507334556036 ) ) ;
#18315 = CARTESIAN_POINT ( 'NONE',  ( 1.749999999999998002, 27.76164181293051669, -4.147968289691384314 ) ) ;
#18316 = EDGE_CURVE ( 'NONE', #15854, #14057, #10726, .T. ) ;
#18317 = DIRECTION ( 'NONE',  ( 0.000000000000000000, 1.000000000000000000, 0.000000000000000000 ) ) ;
#18318 = VERTEX_POINT ( 'NONE', #117 ) ;
#18319 = FACE_OUTER_BOUND ( 'NONE', #7871, .T. ) ;
#18320 = VECTOR ( 'NONE', #11123, 1000.000000000000000 ) ;
#18321 = CARTESIAN_POINT ( 'NONE',  ( 2.695436003842732298, 4.150607464521792522, -10.34374999795161543 ) ) ;
#18322 = ORIENTED_EDGE ( 'NONE', *, *, #14086, .F. ) ;
#18323 = CARTESIAN_POINT ( 'NONE',  ( 11.84374999795161365, -4.888101187500000222, -3.383411828340740850E-14 ) ) ;
#18324 = CARTESIAN_POINT ( 'NONE',  ( 13.86923836996420789, -11.47363181547641453, 35.00000000000000000 ) ) ;
#18325 = ORIENTED_EDGE ( 'NONE', *, *, #3982, .F. ) ;
#18326 = VECTOR ( 'NONE', #13398, 1000.000000000000000 ) ;
#18327 = CARTESIAN_POINT ( 'NONE',  ( 1.510506337161861223, 4.648860486681953397, -12.46874999795161543 ) ) ;
#18328 = EDGE_CURVE ( 'NONE', #8447, #2096, #12228, .T. ) ;
#18329 = CARTESIAN_POINT ( 'NONE',  ( 2.789999999999999147, -15.04425356660744839, -20.70663861606288236 ) ) ;
#18330 = ORIENTED_EDGE ( 'NONE', *, *, #5666, .F. ) ;
#18331 = CARTESIAN_POINT ( 'NONE',  ( 13.84374999795161543, -0.5109457054261775655, 4.861323657744407001 ) ) ;
#18332 = LINE ( 'NONE', #6012, #18977 ) ;
#18333 = VERTEX_POINT ( 'NONE', #4321 ) ;
#18334 = CYLINDRICAL_SURFACE ( 'NONE', #13413, 1.000000000000002665 ) ;
#18335 = VERTEX_POINT ( 'NONE', #10823 ) ;
#18336 = CARTESIAN_POINT ( 'NONE',  ( 13.32184790671640151, 13.12143529358541016, 35.00000000000000000 ) ) ;
#18337 = ORIENTED_EDGE ( 'NONE', *, *, #16739, .F. ) ;
#18338 = FACE_OUTER_BOUND ( 'NONE', #1531, .T. ) ;
#18339 = ADVANCED_FACE ( 'NONE', ( #15027 ), #15718, .T. ) ;
#18340 = CIRCLE ( 'NONE', #467, 5.400000000000000355 ) ;
#18341 = DIRECTION ( 'NONE',  ( 1.000000000000000000, 0.000000000000000000, 0.000000000000000000 ) ) ;
#18342 = LINE ( 'NONE', #4632, #18511 ) ;
#18343 = DIRECTION ( 'NONE',  ( -1.000000000000000000, -0.000000000000000000, -0.000000000000000000 ) ) ;
#18344 = CARTESIAN_POINT ( 'NONE',  ( 6.468749997951615427, 4.233219804643887585, -2.444050593749990341 ) ) ;
#18345 = ORIENTED_EDGE ( 'NONE', *, *, #5053, .F. ) ;
#18346 = DIRECTION ( 'NONE',  ( -0.9135454576425999784, 0.4067366430758019846, 0.000000000000000000 ) ) ;
#18347 = COLOUR_RGB ( '', 0.31764706, 0.68627451, 0.89019608) ;
#18348 = VECTOR ( 'NONE', #9083, 1000.000000000000000 ) ;
#18349 = ORIENTED_EDGE ( 'NONE', *, *, #13292, .F. ) ;
#18350 = VECTOR ( 'NONE', #18525, 1000.000000000000000 ) ;
#18351 = CARTESIAN_POINT ( 'NONE',  ( -36.00000000000000000, 4.999999999999999112, 5.000000000000000000 ) ) ;
#18352 = EDGE_CURVE ( 'NONE', #13049, #12690, #11559, .T. ) ;
#18353 = DIRECTION ( 'NONE',  ( 0.000000000000000000, 0.000000000000000000, -1.000000000000000000 ) ) ;
#18354 = EDGE_LOOP ( 'NONE', ( #17075, #17995, #14336, #19652 ) ) ;
#18355 = CARTESIAN_POINT ( 'NONE',  ( -4.476417968967385974, 17.43449690031536292, 32.00000000000000000 ) ) ;
#18356 = DIRECTION ( 'NONE',  ( 1.000000000000000000, 0.000000000000000000, 0.000000000000000000 ) ) ;
#18357 = CARTESIAN_POINT ( 'NONE',  ( 2.789999999999999147, -12.59161484032927092, 21.30679549418627161 ) ) ;
#18358 = ORIENTED_EDGE ( 'NONE', *, *, #9382, .F. ) ;
#18359 = CARTESIAN_POINT ( 'NONE',  ( 0.5109457054261784537, 4.861323657744407001, -8.468749997951615427 ) ) ;
#18360 = EDGE_CURVE ( 'NONE', #17134, #19326, #18276, .T. ) ;
#18361 = ORIENTED_EDGE ( 'NONE', *, *, #19424, .T. ) ;
#18362 = APPLICATION_PROTOCOL_DEFINITION ( 'draft international standard', 'automotive_design', 1998, #9069 ) ;
#18363 = FACE_OUTER_BOUND ( 'NONE', #1878, .T. ) ;
#18364 = CARTESIAN_POINT ( 'NONE',  ( 6.656249997951614539, -4.233219804643852946, -2.444050593750049849 ) ) ;
#18365 = ORIENTED_EDGE ( 'NONE', *, *, #4801, .T. ) ;
#18366 = VERTEX_POINT ( 'NONE', #9228 ) ;
#18367 = EDGE_CURVE ( 'NONE', #3069, #7195, #14759, .T. ) ;
#18368 = CARTESIAN_POINT ( 'NONE',  ( 0.1882238552569852619, 10.68696068830407420, 23.64332819722385182 ) ) ;
#18369 = CARTESIAN_POINT ( 'NONE',  ( 3.143139765844622957, 4.840010801796481132, -10.81249999590322375 ) ) ;
#18370 = ORIENTED_EDGE ( 'NONE', *, *, #2179, .T. ) ;
#18371 = SURFACE_STYLE_USAGE ( .BOTH. , #12272 ) ;
#18372 = ADVANCED_FACE ( 'NONE', ( #13624 ), #6676, .T. ) ;
#18373 =( GEOMETRIC_REPRESENTATION_CONTEXT ( 3 ) GLOBAL_UNCERTAINTY_ASSIGNED_CONTEXT ( ( #17795 ) ) GLOBAL_UNIT_ASSIGNED_CONTEXT ( ( #9346, #9148, #1542 ) ) REPRESENTATION_CONTEXT ( 'NONE', 'WORKASPACE' ) );
#18374 = ORIENTED_EDGE ( 'NONE', *, *, #4002, .F. ) ;
#18375 = EDGE_CURVE ( 'NONE', #4959, #3602, #1721, .T. ) ;
#18376 = PLANE ( 'NONE',  #18303 ) ;
#18377 = LINE ( 'NONE', #9762, #13230 ) ;
#18378 = CARTESIAN_POINT ( 'NONE',  ( -1.761396867937238042, -5.421022142882365280, -13.31249999590322730 ) ) ;
#18379 = ORIENTED_EDGE ( 'NONE', *, *, #7851, .F. ) ;
#18380 = ORIENTED_EDGE ( 'NONE', *, *, #11763, .T. ) ;
#18381 = DIRECTION ( 'NONE',  ( 0.000000000000000000, 0.9510565162951498674, 0.3090169943749583870 ) ) ;
#18382 = DIRECTION ( 'NONE',  ( 1.000000000000000000, -1.776356839400250465E-15, 0.000000000000000000 ) ) ;
#18383 = ORIENTED_EDGE ( 'NONE', *, *, #18513, .F. ) ;
#18384 = CARTESIAN_POINT ( 'NONE',  ( 2.783068961317272993, 12.53626894672858683, -21.08061549536601476 ) ) ;
#18385 = VECTOR ( 'NONE', #3778, 1000.000000000000000 ) ;
#18386 = FACE_OUTER_BOUND ( 'NONE', #361, .T. ) ;
#18387 = EDGE_CURVE ( 'NONE', #10556, #11614, #2883, .T. ) ;
#18388 = CYLINDRICAL_SURFACE ( 'NONE', #7660, 7.500000000000000000 ) ;
#18389 = CIRCLE ( 'NONE', #9781, 28.06981291497571362 ) ;
#18390 = CARTESIAN_POINT ( 'NONE',  ( 2.071132347512118166, 24.19190980169967631, 12.96989951879416658 ) ) ;
#18391 = CARTESIAN_POINT ( 'NONE',  ( -3.114526743279308896, -3.846120219227901149, -7.343749997951615427 ) ) ;
#18392 = VERTEX_POINT ( 'NONE', #18619 ) ;
#18393 = DIRECTION ( 'NONE',  ( 1.000000000000000000, 0.000000000000000000, -0.000000000000000000 ) ) ;
#18394 = EDGE_CURVE ( 'NONE', #18274, #2041, #17424, .T. ) ;
#18395 = EDGE_LOOP ( 'NONE', ( #6354, #16134, #2100, #12289 ) ) ;
#18396 = CARTESIAN_POINT ( 'NONE',  ( 13.00000000000000533, 5.207209108562852684, -2.318398865532001363 ) ) ;
#18397 = CARTESIAN_POINT ( 'NONE',  ( 9.343749997951615427, -4.780397808154247308, -1.280903732194487166 ) ) ;
#18398 = EDGE_CURVE ( 'NONE', #1264, #3846, #12521, .T. ) ;
#18399 = CIRCLE ( 'NONE', #1152, 0.9999999999999974465 ) ;
#18400 = AXIS2_PLACEMENT_3D ( 'NONE', #19131, #17828, #1122 ) ;
#18401 = CARTESIAN_POINT ( 'NONE',  ( 10.96874999795161720, 1.773574444220789914, -4.620319390059805187 ) ) ;
#18402 = CARTESIAN_POINT ( 'NONE',  ( 2.790000000000000036, -23.69843731927165109, -5.456805104201351675 ) ) ;
#18403 = ORIENTED_EDGE ( 'NONE', *, *, #5425, .T. ) ;
#18404 = DIRECTION ( 'NONE',  ( 0.000000000000000000, 0.000000000000000000, 1.000000000000000000 ) ) ;
#18405 = FACE_OUTER_BOUND ( 'NONE', #4955, .T. ) ;
#18406 = DIRECTION ( 'NONE',  ( 1.000000000000000000, 0.000000000000000000, 0.000000000000000000 ) ) ;
#18407 = VERTEX_POINT ( 'NONE', #11020 ) ;
#18408 = CARTESIAN_POINT ( 'NONE',  ( 1.039999999999997593, 0.000000000000000000, 0.000000000000000000 ) ) ;
#18409 = CARTESIAN_POINT ( 'NONE',  ( 8.468749997951615427, 1.988169868018562436, 4.465502636338039011 ) ) ;
#18410 = CARTESIAN_POINT ( 'NONE',  ( 11.50000000000000355, 2.068159791354184041, 5.387740456496232788 ) ) ;
#18411 = DIRECTION ( 'NONE',  ( 0.000000000000000000, 0.000000000000000000, 1.000000000000000000 ) ) ;
#18412 = ORIENTED_EDGE ( 'NONE', *, *, #11282, .F. ) ;
#18413 = DIRECTION ( 'NONE',  ( 0.000000000000000000, 0.000000000000000000, 1.000000000000000000 ) ) ;
#18414 = B_SPLINE_CURVE_WITH_KNOTS ( 'NONE', 3,
 ( #1688, #1880, #6457, #15301, #13992, #9291 ),
 .UNSPECIFIED., .F., .F.,
 ( 4, 2, 4 ),
 ( 1.979325885387340151E-07, 0.001878588715165610589, 0.003756979497742682708 ),
 .UNSPECIFIED. ) ;
#18415 = CARTESIAN_POINT ( 'NONE',  ( -2.444050593749990785, 4.233219804643887585, -6.843749997951615427 ) ) ;
#18416 = AXIS2_PLACEMENT_3D ( 'NONE', #1074, #8279, #14498 ) ;
#18417 = VERTEX_POINT ( 'NONE', #18520 ) ;
#18418 = DIRECTION ( 'NONE',  ( 0.000000000000000000, -1.000000000000000000, 0.000000000000000000 ) ) ;
#18419 = DIRECTION ( 'NONE',  ( 0.000000000000000000, 0.000000000000000000, 1.000000000000000000 ) ) ;
#18420 = VERTEX_POINT ( 'NONE', #2108 ) ;
#18421 = EDGE_CURVE ( 'NONE', #15138, #1129, #19223, .T. ) ;
#18422 = CARTESIAN_POINT ( 'NONE',  ( 3.499494075959815653, 3.499494075959816541, -13.96874999795161365 ) ) ;
#18423 = DIRECTION ( 'NONE',  ( -1.000000000000000000, -0.000000000000000000, -0.000000000000000000 ) ) ;
#18424 = ORIENTED_EDGE ( 'NONE', *, *, #17234, .F. ) ;
#18425 = VECTOR ( 'NONE', #11196, 1000.000000000000000 ) ;
#18426 = CARTESIAN_POINT ( 'NONE',  ( 0.000000000000000000, 0.000000000000000000, 29.00000000000000355 ) ) ;
#18427 = PLANE ( 'NONE',  #3018 ) ;
#18428 = AXIS2_PLACEMENT_3D ( 'NONE', #1976, #14185, #6559 ) ;
#18429 = ORIENTED_EDGE ( 'NONE', *, *, #163, .T. ) ;
#18430 = DIRECTION ( 'NONE',  ( 1.000000000000000000, 0.000000000000000000, 0.000000000000000000 ) ) ;
#18431 = ORIENTED_EDGE ( 'NONE', *, *, #11774, .F. ) ;
#18432 = DIRECTION ( 'NONE',  ( -1.000000000000000000, -0.000000000000000000, -0.000000000000000000 ) ) ;
#18433 = VERTEX_POINT ( 'NONE', #9624 ) ;
#18434 = EDGE_CURVE ( 'NONE', #3616, #2009, #16347, .T. ) ;
#18435 = DIRECTION ( 'NONE',  ( 1.000000000000000000, 0.000000000000000000, 0.000000000000000000 ) ) ;
#18436 = DIRECTION ( 'NONE',  ( -1.000000000000000000, -6.419766481290786633E-33, 0.000000000000000000 ) ) ;
#18437 = CARTESIAN_POINT ( 'NONE',  ( 2.789999999999999147, 2.680914349914567470E-13, -25.59481291497571220 ) ) ;
#18438 = CARTESIAN_POINT ( 'NONE',  ( 1.039999999999998925, -4.147968289691484678, 27.76164181293050248 ) ) ;
#18439 = ORIENTED_EDGE ( 'NONE', *, *, #17494, .T. ) ;
#18440 = CARTESIAN_POINT ( 'NONE',  ( 0.06555561860988173839, 21.84113606038307509, 12.72236714503170596 ) ) ;
#18441 =( BOUNDED_CURVE ( )  B_SPLINE_CURVE ( 2, ( #8504, #18805, #513, #6581, #2001 ),
 .UNSPECIFIED., .F., .F. ) 
 B_SPLINE_CURVE_WITH_KNOTS ( ( 3, 2, 3 ),
 ( 0.3333180920165872418, 0.3499999999999999778, 0.4000000000000000222 ),
 .UNSPECIFIED. ) 
 CURVE ( )  GEOMETRIC_REPRESENTATION_ITEM ( )  RATIONAL_B_SPLINE_CURVE ( ( 0.9945256517182510247, 0.9958923606136993456, 1.000000000000000000, 0.9876883405951377704, 1.000000000000000000 ) ) 
 REPRESENTATION_ITEM ( '' )  );
#18442 = VECTOR ( 'NONE', #18286, 1000.000000000000000 ) ;
#18443 = FACE_OUTER_BOUND ( 'NONE', #14195, .T. ) ;
#18444 = ORIENTED_EDGE ( 'NONE', *, *, #11467, .F. ) ;
#18445 = EDGE_CURVE ( 'NONE', #19252, #3827, #15624, .T. ) ;
#18446 = CARTESIAN_POINT ( 'NONE',  ( 12.99999999999969624, 3.863910152777037421, -3.836387901770561104 ) ) ;
#18447 = CARTESIAN_POINT ( 'NONE',  ( 2.789999999999999147, 0.000000000000000000, 0.000000000000000000 ) ) ;
#18448 = ORIENTED_EDGE ( 'NONE', *, *, #17032, .F. ) ;
#18449 = CYLINDRICAL_SURFACE ( 'NONE', #13234, 1.000000000000004441 ) ;
#18450 = CARTESIAN_POINT ( 'NONE',  ( -19.00000000000000355, 4.898587196589412829E-16, 0.000000000000000000 ) ) ;
#18451 = VERTEX_POINT ( 'NONE', #11324 ) ;
#18452 = CARTESIAN_POINT ( 'NONE',  ( 1.749999999999998002, -25.12109765559643648, -12.52377138324252570 ) ) ;
#18453 = AXIS2_PLACEMENT_3D ( 'NONE', #14431, #11615, #11712 ) ;
#18454 = ORIENTED_EDGE ( 'NONE', *, *, #11619, .F. ) ;
#18455 = CARTESIAN_POINT ( 'NONE',  ( -6.929096493834647319, 2.870125742738179664, 12.00000000000000000 ) ) ;
#18456 = CIRCLE ( 'NONE', #10469, 2.524999999999995914 ) ;
#18457 = FILL_AREA_STYLE ('',( #7541 ) ) ;
#18458 = VERTEX_POINT ( 'NONE', #415 ) ;
#18459 = ORIENTED_EDGE ( 'NONE', *, *, #10114, .F. ) ;
#18460 = DIRECTION ( 'NONE',  ( -0.000000000000000000, 0.000000000000000000, 1.000000000000000000 ) ) ;
#18461 = B_SPLINE_CURVE_WITH_KNOTS ( 'NONE', 3,
 ( #9144, #10544, #135, #15250, #19534, #18438 ),
 .UNSPECIFIED., .F., .F.,
 ( 4, 2, 4 ),
 ( 2.132675795041204291E-07, 0.001878604073277003036, 0.003756994878974502169 ),
 .UNSPECIFIED. ) ;
#18462 = CARTESIAN_POINT ( 'NONE',  ( 4.781284448697195266, 1.016293382781411792, -12.84374999795161543 ) ) ;
#18463 = ORIENTED_EDGE ( 'NONE', *, *, #16725, .T. ) ;
#18464 = ADVANCED_FACE ( 'NONE', ( #13923, #8004 ), #6693, .F. ) ;
#18465 = EDGE_CURVE ( 'NONE', #6403, #8156, #3415, .T. ) ;
#18466 = FACE_OUTER_BOUND ( 'NONE', #13805, .T. ) ;
#18467 = CIRCLE ( 'NONE', #4415, 1.000000000000002665 ) ;
#18468 = EDGE_LOOP ( 'NONE', ( #13268, #1711, #15661, #12642 ) ) ;
#18469 = AXIS2_PLACEMENT_3D ( 'NONE', #110, #7292, #13515 ) ;
#18470 = FACE_OUTER_BOUND ( 'NONE', #11334, .T. ) ;
#18471 = CARTESIAN_POINT ( 'NONE',  ( -7.595268335593441642E-14, -22.38018801136484015, 9.515416771311118183 ) ) ;
#18472 = DIRECTION ( 'NONE',  ( 0.000000000000000000, 0.000000000000000000, -1.000000000000000000 ) ) ;
#18473 = CARTESIAN_POINT ( 'NONE',  ( 2.789999999999999147, 0.000000000000000000, 0.000000000000000000 ) ) ;
#18474 = ORIENTED_EDGE ( 'NONE', *, *, #17608, .F. ) ;
#18475 = ORIENTED_EDGE ( 'NONE', *, *, #6140, .T. ) ;
#18476 = CARTESIAN_POINT ( 'NONE',  ( -1.899999999999999023, 0.000000000000000000, -8.239200000000002078 ) ) ;
#18477 = CYLINDRICAL_SURFACE ( 'NONE', #13809, 13.19999999999999929 ) ;
#18478 = ORIENTED_EDGE ( 'NONE', *, *, #11474, .T. ) ;
#18479 = ORIENTED_EDGE ( 'NONE', *, *, #18352, .T. ) ;
#18480 = CARTESIAN_POINT ( 'NONE',  ( -11.00000000000000355, -4.898587196589412829E-16, 0.000000000000000000 ) ) ;
#18481 = CIRCLE ( 'NONE', #288, 1.000000000000004441 ) ;
#18482 = DIRECTION ( 'NONE',  ( 0.000000000000000000, 0.000000000000000000, -1.000000000000000000 ) ) ;
#18483 = CARTESIAN_POINT ( 'NONE',  ( 0.02436607992776151574, -16.37294372382871188, 18.55949924794887096 ) ) ;
#18484 = CARTESIAN_POINT ( 'NONE',  ( -2.000000000000000000, -2.000000000000002665, 37.99999999999999289 ) ) ;
#18485 = CARTESIAN_POINT ( 'NONE',  ( -0.5958122406255597081, 5.668774803599165857, -15.31249999590322552 ) ) ;
#18486 = VERTEX_POINT ( 'NONE', #15821 ) ;
#18487 = CARTESIAN_POINT ( 'NONE',  ( 9.343749997951615427, -1.280903732194386579, -4.780397808154273953 ) ) ;
#18488 = CARTESIAN_POINT ( 'NONE',  ( 7.843749997951614539, -1.510506337161893864, 4.648860486681943627 ) ) ;
#18489 = VERTEX_POINT ( 'NONE', #3612 ) ;
#18490 = DIRECTION ( 'NONE',  ( 1.000000000000000000, 0.000000000000000000, 0.000000000000000000 ) ) ;
#18491 = EDGE_CURVE ( 'NONE', #11541, #12253, #18913, .T. ) ;
#18492 = EDGE_CURVE ( 'NONE', #12097, #11096, #10922, .T. ) ;
#18493 = CARTESIAN_POINT ( 'NONE',  ( 7.937500000000000000, 4.582717761692664205, -0.7089489049740167470 ) ) ;
#18494 = AXIS2_PLACEMENT_3D ( 'NONE', #1437, #1535, #7623 ) ;
#18495 = FACE_OUTER_BOUND ( 'NONE', #3234, .T. ) ;
#18496 = CARTESIAN_POINT ( 'NONE',  ( 15.19790265903627358, 9.644882309621939598, 35.00000000000000000 ) ) ;
#18497 = VERTEX_POINT ( 'NONE', #521 ) ;
#18498 = CARTESIAN_POINT ( 'NONE',  ( -90.00000000000000000, 0.000000000000000000, 0.000000000000000000 ) ) ;
#18499 = FILL_AREA_STYLE_COLOUR ( '', #8100 ) ;
#18500 = CARTESIAN_POINT ( 'NONE',  ( 0.5321745227542249435, 18.57583492944418779, 19.66801664102709779 ) ) ;
#18501 = PRODUCT_DEFINITION_FORMATION_WITH_SPECIFIED_SOURCE ( 'ANY', '', #2666, .NOT_KNOWN. ) ;
#18502 = EDGE_CURVE ( 'NONE', #6506, #14054, #15392, .T. ) ;
#18503 = CARTESIAN_POINT ( 'NONE',  ( 0.000000000000000000, 0.000000000000000000, 0.000000000000000000 ) ) ;
#18504 = ORIENTED_EDGE ( 'NONE', *, *, #2295, .T. ) ;
#18505 = CARTESIAN_POINT ( 'NONE',  ( 5.700000000000001066, -4.360680574150373717E-16, -12.66727757604273386 ) ) ;
#18506 = CYLINDRICAL_SURFACE ( 'NONE', #7431, 6.735000000000022524 ) ;
#18507 = CARTESIAN_POINT ( 'NONE',  ( 2.318398865532038666, -5.207209108562836697, -13.00000000000000533 ) ) ;
#18508 = DIRECTION ( 'NONE',  ( 0.000000000000000000, 0.000000000000000000, -1.000000000000000000 ) ) ;
#18509 = EDGE_LOOP ( 'NONE', ( #11058, #44 ) ) ;
#18510 = DIRECTION ( 'NONE',  ( 1.000000000000000000, 1.224646799147353207E-16, 0.000000000000000000 ) ) ;
#18511 = VECTOR ( 'NONE', #11310, 1000.000000000000000 ) ;
#18512 = CARTESIAN_POINT ( 'NONE',  ( -2.873153789725825469, 3.954556930911862000, -9.843749997951615427 ) ) ;
#18513 = EDGE_CURVE ( 'NONE', #1230, #4750, #7811, .T. ) ;
#18514 = VERTEX_POINT ( 'NONE', #9429 ) ;
#18515 = CARTESIAN_POINT ( 'NONE',  ( 6.968749997951614539, -0.7741991708319229115, 4.888101187499994893 ) ) ;
#18516 = DIRECTION ( 'NONE',  ( 0.000000000000000000, 0.000000000000000000, -1.000000000000000000 ) ) ;
#18517 = CIRCLE ( 'NONE', #11846, 6.000000000000000000 ) ;
#18518 = EDGE_LOOP ( 'NONE', ( #19301, #10687, #10874, #15362 ) ) ;
#18519 = EDGE_CURVE ( 'NONE', #16090, #19316, #1646, .T. ) ;
#18520 = CARTESIAN_POINT ( 'NONE',  ( 6.000000000000005329, 0.000000000000000000, -5.700000000000001066 ) ) ;
#18521 = CARTESIAN_POINT ( 'NONE',  ( 1.886022603841227330, 0.000000000000000000, -8.265000000000021885 ) ) ;
#18522 = ORIENTED_EDGE ( 'NONE', *, *, #11013, .T. ) ;
#18523 = B_SPLINE_CURVE_WITH_KNOTS ( 'NONE', 3,
 ( #3541, #12362, #3643, #3348 ),
 .UNSPECIFIED., .F., .F.,
 ( 4, 4 ),
 ( 0.0006045424356928436873, 0.0006887909409525051459 ),
 .UNSPECIFIED. ) ;
#18524 = DIRECTION ( 'NONE',  ( 1.000000000000000000, 0.000000000000000000, 0.000000000000000000 ) ) ;
#18525 = DIRECTION ( 'NONE',  ( 0.8660254037844380415, -0.5000000000000009992, 0.000000000000000000 ) ) ;
#18526 = EDGE_CURVE ( 'NONE', #10900, #11655, #6495, .T. ) ;
#18527 = VERTEX_POINT ( 'NONE', #12624 ) ;
#18528 = CARTESIAN_POINT ( 'NONE',  ( 0.000000000000000000, 0.000000000000000000, 12.00000000000000000 ) ) ;
#18529 = ORIENTED_EDGE ( 'NONE', *, *, #16300, .T. ) ;
#18530 = CARTESIAN_POINT ( 'NONE',  ( -4.888101187500000222, 0.000000000000000000, -6.843749997951615427 ) ) ;
#18531 = EDGE_LOOP ( 'NONE', ( #17035, #11602, #315, #18817 ) ) ;
#18532 = CARTESIAN_POINT ( 'NONE',  ( -15.00000000000000355, 4.215373648918916416, -3.375000000000002665 ) ) ;
#18533 = PLANE ( 'NONE',  #9177 ) ;
#18534 = CARTESIAN_POINT ( 'NONE',  ( -2.850000000000058265, -4.936344801571268093, -6.000000000000005329 ) ) ;
#18535 = ADVANCED_FACE ( 'NONE', ( #7906 ), #4845, .T. ) ;
#18536 = CARTESIAN_POINT ( 'NONE',  ( 2.789999999999999147, 7.909232158574813099, 24.34211360614303388 ) ) ;
#18537 = VERTEX_POINT ( 'NONE', #14021 ) ;
#18538 = DIRECTION ( 'NONE',  ( 0.000000000000000000, 1.224646799147353947E-16, 1.000000000000000000 ) ) ;
#18539 = CARTESIAN_POINT ( 'NONE',  ( 0.000000000000000000, 7.909232158575156824, -24.34211360614291664 ) ) ;
#18540 = AXIS2_PLACEMENT_3D ( 'NONE', #1581, #7669, #13753 ) ;
#18541 = ORIENTED_EDGE ( 'NONE', *, *, #16910, .F. ) ;
#18542 = CIRCLE ( 'NONE', #11831, 8.265000000000021885 ) ;
#18543 = LINE ( 'NONE', #18351, #4508 ) ;
#18544 = CARTESIAN_POINT ( 'NONE',  ( -4.999999999999966249, -7.196152422706654228, 37.99999999999999289 ) ) ;
#18545 = VERTEX_POINT ( 'NONE', #2011 ) ;
#18546 = DIRECTION ( 'NONE',  ( -1.000000000000000000, -0.000000000000000000, -0.000000000000000000 ) ) ;
#18547 = FACE_OUTER_BOUND ( 'NONE', #2153, .T. ) ;
#18548 = EDGE_LOOP ( 'NONE', ( #7845, #687, #698, #16023 ) ) ;
#18549 = CARTESIAN_POINT ( 'NONE',  ( -17.28688694438836393, -7.664027248171298545, -32.00000000000000000 ) ) ;
#18550 = ADVANCED_FACE ( 'NONE', ( #2492 ), #9974, .T. ) ;
#18551 = ORIENTED_EDGE ( 'NONE', *, *, #2051, .F. ) ;
#18552 = APPLICATION_PROTOCOL_DEFINITION ( 'draft international standard', 'automotive_design', 1998, #9450 ) ;
#18553 = LINE ( 'NONE', #5244, #13824 ) ;
#18554 = CYLINDRICAL_SURFACE ( 'NONE', #3218, 9.000000000000001776 ) ;
#18555 = ORIENTED_EDGE ( 'NONE', *, *, #9215, .T. ) ;
#18556 =( BOUNDED_SURFACE ( )  B_SPLINE_SURFACE ( 1, 2, ( 
 ( #16631, #9130, #15236, #1427, #1527, #8929, #9028, #11830, #7403, #13328, #5814, #7612, #18237, #4515, #6011, #7508, #2911 ),
 ( #17939, #13726, #12232, #10632, #11930, #3016, #12134, #16737, #16335, #13423, #7303, #4327, #18, #19429, #18331, #19630, #13528 ) ),
 .UNSPECIFIED., .F., .F., .F. ) 
 B_SPLINE_SURFACE_WITH_KNOTS ( ( 2, 2 ),
 ( 3, 2, 2, 2, 2, 2, 2, 2, 3 ),
 ( 0.000000000000000000, 1.000000000000000000 ),
 ( 0.000000000000000000, 0.05000000000000000278, 0.1000000000000000056, 0.1499999999999999944, 0.2000000000000000111, 0.2500000000000000000, 0.2999999999999999889, 0.3499999999999999778, 0.4000000000000000222 ),
 .UNSPECIFIED. ) 
 GEOMETRIC_REPRESENTATION_ITEM ( )  RATIONAL_B_SPLINE_SURFACE ( (
 ( 1.000000000000000000, 0.9876883405951377704, 1.000000000000000000, 0.9876883405951377704, 1.000000000000000000, 0.9876883405951377704, 1.000000000000000000, 0.9876883405951377704, 1.000000000000000000, 0.9876883405951377704, 1.000000000000000000, 0.9876883405951377704, 1.000000000000000000, 0.9876883405951377704, 1.000000000000000000, 0.9876883405951377704, 1.000000000000000000),
 ( 1.000000000000000000, 0.9876883405951377704, 1.000000000000000000, 0.9876883405951377704, 1.000000000000000000, 0.9876883405951377704, 1.000000000000000000, 0.9876883405951377704, 1.000000000000000000, 0.9876883405951377704, 1.000000000000000000, 0.9876883405951377704, 1.000000000000000000, 0.9876883405951377704, 1.000000000000000000, 0.9876883405951377704, 1.000000000000000000) ) ) 
 REPRESENTATION_ITEM ( '' )  SURFACE ( )  );
#18557 = ORIENTED_EDGE ( 'NONE', *, *, #11534, .T. ) ;
#18558 = LINE ( 'NONE', #9366, #17199 ) ;
#18559 = VECTOR ( 'NONE', #8900, 1000.000000000000227 ) ;
#18560 =( REPRESENTATION_RELATIONSHIP ('NONE','NONE', #18211, #451 ) REPRESENTATION_RELATIONSHIP_WITH_TRANSFORMATION ( #8347 )SHAPE_REPRESENTATION_RELATIONSHIP( ) );
#18561 = LINE ( 'NONE', #8966, #2466 ) ;
#18562 = EDGE_CURVE ( 'NONE', #19081, #4439, #6424, .T. ) ;
#18563 = ORIENTED_EDGE ( 'NONE', *, *, #4692, .T. ) ;
#18564 = CYLINDRICAL_SURFACE ( 'NONE', #6760, 0.9999999999999974465 ) ;
#18565 = VERTEX_POINT ( 'NONE', #19201 ) ;
#18566 = AXIS2_PLACEMENT_3D ( 'NONE', #11241, #6617, #17447 ) ;
#18567 = CARTESIAN_POINT ( 'NONE',  ( -20.63749999999999929, 0.000000000000000000, 0.000000000000000000 ) ) ;
#18568 = AXIS2_PLACEMENT_3D ( 'NONE', #9240, #2824, #1331 ) ;
#18569 = CARTESIAN_POINT ( 'NONE',  ( 2.789999999999999147, 15.04425356660790136, -20.70663861606255196 ) ) ;
#18570 = ADVANCED_FACE ( 'NONE', ( #5308 ), #17634, .T. ) ;
#18571 = CARTESIAN_POINT ( 'NONE',  ( 2.604434283110813375, -12.84444904262041121, 22.53097606932980312 ) ) ;
#18572 = ORIENTED_EDGE ( 'NONE', *, *, #14706, .T. ) ;
#18573 = FACE_BOUND ( 'NONE', #17770, .T. ) ;
#18574 = DIRECTION ( 'NONE',  ( 0.000000000000000000, 0.000000000000000000, 1.000000000000000000 ) ) ;
#18575 = VERTEX_POINT ( 'NONE', #11608 ) ;
#18576 = ORIENTED_EDGE ( 'NONE', *, *, #9986, .F. ) ;
#18577 = CARTESIAN_POINT ( 'NONE',  ( 2.257825462012207129, -12.96514671151749631, -23.74442027961374890 ) ) ;
#18578 = CARTESIAN_POINT ( 'NONE',  ( -0.5958122406256771697, -5.668774803599153422, -9.312499995903225525 ) ) ;
#18579 = CARTESIAN_POINT ( 'NONE',  ( -6.626241948324210540, -16.73597674598852336, 35.00000000000000000 ) ) ;
#18580 = ADVANCED_FACE ( 'NONE', ( #14810 ), #9674, .T. ) ;
#18581 = CARTESIAN_POINT ( 'NONE',  ( 5.510910596163084625E-16, 18.00000000000000355, 35.00000000000000000 ) ) ;
#18582 = AXIS2_PLACEMENT_3D ( 'NONE', #313, #6392, #9731 ) ;
#18583 = CARTESIAN_POINT ( 'NONE',  ( -4.780397808154273953, -1.280903732194386579, -9.343749997951615427 ) ) ;
#18584 = ORIENTED_EDGE ( 'NONE', *, *, #16191, .T. ) ;
#18585 = CARTESIAN_POINT ( 'NONE',  ( 0.000000000000000000, 0.000000000000000000, 0.000000000000000000 ) ) ;
#18586 = CARTESIAN_POINT ( 'NONE',  ( 0.000000000000000000, -9.324097380959594616, 22.25075486061734509 ) ) ;
#18587 = VERTEX_POINT ( 'NONE', #17614 ) ;
#18588 = CARTESIAN_POINT ( 'NONE',  ( -8.776855558857221240, 3.635492607468361115, 12.00000000000000000 ) ) ;
#18589 = CARTESIAN_POINT ( 'NONE',  ( -90.00000000000000000, 0.000000000000000000, 0.000000000000000000 ) ) ;
#18590 = DIRECTION ( 'NONE',  ( 0.000000000000000000, 0.000000000000000000, 1.000000000000000000 ) ) ;
#18591 = CARTESIAN_POINT ( 'NONE',  ( 2.789999999999999147, -19.91106274590503844, -14.18181402625762821 ) ) ;
#18592 = EDGE_CURVE ( 'NONE', #11187, #15562, #12540, .T. ) ;
#18593 = DIRECTION ( 'NONE',  ( 1.000000000000000000, 0.000000000000000000, 0.000000000000000000 ) ) ;
#18594 = VERTEX_POINT ( 'NONE', #5688 ) ;
#18595 = VECTOR ( 'NONE', #13722, 1000.000000000000000 ) ;
#18596 = CIRCLE ( 'NONE', #2625, 0.9999999999999974465 ) ;
#18597 = DIRECTION ( 'NONE',  ( 0.000000000000000000, 0.7315216790650492795, -0.6818181818181815457 ) ) ;
#18598 = FACE_OUTER_BOUND ( 'NONE', #14631, .T. ) ;
#18599 = CIRCLE ( 'NONE', #3904, 2.524999999999996358 ) ;
#18600 = CARTESIAN_POINT ( 'NONE',  ( -17.96448111170888851, 1.130229351527647585, -35.00000000000000000 ) ) ;
#18601 = EDGE_LOOP ( 'NONE', ( #14350, #516, #19368, #11739 ) ) ;
#18602 = DIRECTION ( 'NONE',  ( 0.000000000000000000, 0.000000000000000000, 1.000000000000000000 ) ) ;
#18603 = CARTESIAN_POINT ( 'NONE',  ( 13.96874999795161365, -1.280903732194453859, 4.780397808154257078 ) ) ;
#18604 = AXIS2_PLACEMENT_3D ( 'NONE', #14986, #14891, #19480 ) ;
#18605 = CARTESIAN_POINT ( 'NONE',  ( 10.58013454126452046, -14.56230589874905412, 32.00000000000000000 ) ) ;
#18606 = EDGE_LOOP ( 'NONE', ( #1698, #9612, #15257, #1476, #12504, #10574 ) ) ;
#18607 = ADVANCED_FACE ( 'NONE', ( #5498 ), #11886, .T. ) ;
#18608 = CARTESIAN_POINT ( 'NONE',  ( -2.000000000000001776, 0.000000000000000000, 6.500000000000000000 ) ) ;
#18609 = CARTESIAN_POINT ( 'NONE',  ( -0.7741991708318890497, 4.888101187500000222, -11.34374999795161543 ) ) ;
#18610 = EDGE_LOOP ( 'NONE', ( #5002, #6460, #10731, #5032, #15511 ) ) ;
#18611 = CARTESIAN_POINT ( 'NONE',  ( 10.00000000000000533, 1.185096637661293251, -5.575441324182679459 ) ) ;
#18612 = CARTESIAN_POINT ( 'NONE',  ( 1.039999999999999369, -12.52377138324206918, -25.12109765559666741 ) ) ;
#18613 = ORIENTED_EDGE ( 'NONE', *, *, #11519, .F. ) ;
#18614 = AXIS2_PLACEMENT_3D ( 'NONE', #12049, #18153, #16647 ) ;
#18615 = EDGE_CURVE ( 'NONE', #19204, #10556, #12929, .T. ) ;
#18616 = EDGE_CURVE ( 'NONE', #4963, #18392, #11264, .T. ) ;
#18617 = CLOSED_SHELL ( 'NONE', ( #2130, #1693, #4323, #18282, #12911, #15816, #9922, #3638, #10926, #2933, #8946, #640, #17728, #12028, #6700, #17767, #10455, #6658, #4277, #15568, #17885, #9702, #13108, #8066, #17331, #14317, #5176, #7260, #413, #15017, #7153, #8168, #13924, #19275, #16638, #19650, #14, #371 ) ) ;
#18618 = AXIS2_PLACEMENT_3D ( 'NONE', #4772, #269, #16081 ) ;
#18619 = CARTESIAN_POINT ( 'NONE',  ( -15.00000000000000355, -3.434748899119118626, 2.750000000000001332 ) ) ;
#18620 = DIRECTION ( 'NONE',  ( 0.000000000000000000, 0.000000000000000000, -1.000000000000000000 ) ) ;
#18621 = EDGE_LOOP ( 'NONE', ( #1861, #16770, #151, #1848 ) ) ;
#18622 = CARTESIAN_POINT ( 'NONE',  ( 0.006931069955679173590, 18.43696893154758598, 16.17493693894884998 ) ) ;
#18623 = EDGE_CURVE ( 'NONE', #18417, #18575, #3905, .T. ) ;
#18624 = DIRECTION ( 'NONE',  ( -1.000000000000000000, 0.000000000000000000, -0.000000000000000000 ) ) ;
#18625 = VERTEX_POINT ( 'NONE', #6891 ) ;
#18626 = DIRECTION ( 'NONE',  ( -0.6363829547955638377, 0.000000000000000000, -0.7713732785400770897 ) ) ;
#18627 = VERTEX_POINT ( 'NONE', #1105 ) ;
#18628 = CARTESIAN_POINT ( 'NONE',  ( 4.936344801571289409, -2.850000000000023626, -12.31249999590322552 ) ) ;
#18629 = ORIENTED_EDGE ( 'NONE', *, *, #17974, .T. ) ;
#18630 = CARTESIAN_POINT ( 'NONE',  ( 2.718131864678288601, 2.577209017047007666, 25.22589920183362722 ) ) ;
#18631 = CARTESIAN_POINT ( 'NONE',  ( -4.465502636338010589, 1.988169868018623720, -14.84374999795161543 ) ) ;
#18632 = FACE_OUTER_BOUND ( 'NONE', #8693, .T. ) ;
#18633 = CIRCLE ( 'NONE', #10024, 4.200000000000000178 ) ;
#18634 = DIRECTION ( 'NONE',  ( -1.000000000000000000, -0.000000000000000000, -0.000000000000000000 ) ) ;
#18635 = ORIENTED_EDGE ( 'NONE', *, *, #892, .F. ) ;
#18636 = AXIS2_PLACEMENT_3D ( 'NONE', #6779, #2092, #8195 ) ;
#18637 = DIRECTION ( 'NONE',  ( -1.000000000000000000, -0.000000000000000000, -0.000000000000000000 ) ) ;
#18638 = B_SPLINE_CURVE_WITH_KNOTS ( 'NONE', 3,
 ( #8961, #15162, #7540, #13661, #18266, #4551 ),
 .UNSPECIFIED., .F., .F.,
 ( 4, 2, 4 ),
 ( 4.462636678112536814E-07, 0.001879885020955181143, 0.003759323778242551310 ),
 .UNSPECIFIED. ) ;
#18639 = LINE ( 'NONE', #9546, #12655 ) ;
#18640 = VERTEX_POINT ( 'NONE', #7178 ) ;
#18641 = VERTEX_POINT ( 'NONE', #14420 ) ;
#18642 = DIRECTION ( 'NONE',  ( -0.000000000000000000, -0.000000000000000000, 1.000000000000000000 ) ) ;
#18643 = CYLINDRICAL_SURFACE ( 'NONE', #3940, 3.000000000000000000 ) ;
#18644 = VERTEX_POINT ( 'NONE', #13300 ) ;
#18645 = CARTESIAN_POINT ( 'NONE',  ( 2.718184767880471142, 10.24584646439571500, -23.19431517146922417 ) ) ;
#18646 = DIRECTION ( 'NONE',  ( 0.000000000000000000, 0.000000000000000000, -1.000000000000000000 ) ) ;
#18647 = VECTOR ( 'NONE', #14908, 1000.000000000000000 ) ;
#18648 = ORIENTED_EDGE ( 'NONE', *, *, #19012, .F. ) ;
#18649 = CARTESIAN_POINT ( 'NONE',  ( 2.000000000000000000, 4.999999999999998224, 41.99999999999999289 ) ) ;
#18650 = ORIENTED_EDGE ( 'NONE', *, *, #2202, .F. ) ;
#18651 = APPLICATION_PROTOCOL_DEFINITION ( 'draft international standard', 'automotive_design', 1998, #17367 ) ;
#18652 = DIRECTION ( 'NONE',  ( -0.000000000000000000, -0.000000000000000000, 1.000000000000000000 ) ) ;
#18653 = CARTESIAN_POINT ( 'NONE',  ( 9.968749997951617203, 4.150607464521791634, 2.695436003842732298 ) ) ;
#18654 = ORIENTED_EDGE ( 'NONE', *, *, #13316, .F. ) ;
#18655 = ORIENTED_EDGE ( 'NONE', *, *, #1391, .T. ) ;
#18656 = DIRECTION ( 'NONE',  ( 0.000000000000000000, -1.000000000000000000, 0.000000000000000000 ) ) ;
#18657 = VECTOR ( 'NONE', #15600, 1000.000000000000000 ) ;
#18658 = DIRECTION ( 'NONE',  ( 0.000000000000000000, 0.000000000000000000, -1.000000000000000000 ) ) ;
#18659 = ORIENTED_EDGE ( 'NONE', *, *, #2017, .T. ) ;
#18660 = B_SPLINE_CURVE_WITH_KNOTS ( 'NONE', 3,
 ( #15642, #3528, #10843, #9644 ),
 .UNSPECIFIED., .F., .F.,
 ( 4, 4 ),
 ( 2.034713381942717888E-07, 0.0006887909409525252036 ),
 .UNSPECIFIED. ) ;
#18661 = CARTESIAN_POINT ( 'NONE',  ( -4.780397808154273953, -1.280903732194386579, -9.343749997951615427 ) ) ;
#18662 = CIRCLE ( 'NONE', #16123, 5.700000000000001954 ) ;
#18663 = ORIENTED_EDGE ( 'NONE', *, *, #15814, .T. ) ;
#18664 = CIRCLE ( 'NONE', #7150, 2.524999999999996358 ) ;
#18665 = CARTESIAN_POINT ( 'NONE',  ( -2.300000000000000711, 0.000000000000000000, 0.000000000000000000 ) ) ;
#18666 = EDGE_CURVE ( 'NONE', #13990, #562, #19236, .T. ) ;
#18667 = DIRECTION ( 'NONE',  ( 0.000000000000000000, 0.000000000000000000, -1.000000000000000000 ) ) ;
#18668 =( BOUNDED_SURFACE ( )  B_SPLINE_SURFACE ( 1, 2, ( 
 ( #4998, #4265, #11667, #2751, #5655, #5853, #11865, #2456, #13363, #2094, #17977, #19559, #6680, #13175, #10084, #12804, #18073 ),
 ( #8770, #14772, #11309, #10176, #18901, #14871, #1263, #7340, #19461, #13458, #1067, #1165, #17409, #964, #3694, #4365, #7239 ) ),
 .UNSPECIFIED., .F., .F., .F. ) 
 B_SPLINE_SURFACE_WITH_KNOTS ( ( 2, 2 ),
 ( 3, 2, 2, 2, 2, 2, 2, 2, 3 ),
 ( 0.000000000000000000, 1.000000000000000000 ),
 ( 0.000000000000000000, 0.05000000000000000278, 0.1000000000000000056, 0.1499999999999999944, 0.2000000000000000111, 0.2500000000000000000, 0.2999999999999999889, 0.3499999999999999778, 0.4000000000000000222 ),
 .UNSPECIFIED. ) 
 GEOMETRIC_REPRESENTATION_ITEM ( )  RATIONAL_B_SPLINE_SURFACE ( (
 ( 1.000000000000000000, 0.9876883405951377704, 1.000000000000000000, 0.9876883405951377704, 1.000000000000000000, 0.9876883405951377704, 1.000000000000000000, 0.9876883405951377704, 1.000000000000000000, 0.9876883405951377704, 1.000000000000000000, 0.9876883405951377704, 1.000000000000000000, 0.9876883405951377704, 1.000000000000000000, 0.9876883405951377704, 1.000000000000000000),
 ( 1.000000000000000000, 0.9876883405951377704, 1.000000000000000000, 0.9876883405951377704, 1.000000000000000000, 0.9876883405951377704, 1.000000000000000000, 0.9876883405951377704, 1.000000000000000000, 0.9876883405951377704, 1.000000000000000000, 0.9876883405951377704, 1.000000000000000000, 0.9876883405951377704, 1.000000000000000000, 0.9876883405951377704, 1.000000000000000000) ) ) 
 REPRESENTATION_ITEM ( '' )  SURFACE ( )  );
#18669 = DIRECTION ( 'NONE',  ( -1.000000000000000000, -0.000000000000000000, -0.000000000000000000 ) ) ;
#18670 = ORIENTED_EDGE ( 'NONE', *, *, #18090, .F. ) ;
#18671 = CARTESIAN_POINT ( 'NONE',  ( 0.07186811453410638095, -16.91241718342012490, 18.89333555428548905 ) ) ;
#18672 = PRESENTATION_STYLE_ASSIGNMENT (( #3469 ) ) ;
#18673 = LINE ( 'NONE', #175, #15414 ) ;
#18674 = AXIS2_PLACEMENT_3D ( 'NONE', #19115, #17716, #7183 ) ;
#18675 = B_SPLINE_CURVE_WITH_KNOTS ( 'NONE', 3,
 ( #14172, #15676, #17842, #1136 ),
 .UNSPECIFIED., .F., .F.,
 ( 4, 4 ),
 ( 0.000000000000000000, 0.001126652051248518355 ),
 .UNSPECIFIED. ) ;
#18676 = VERTEX_POINT ( 'NONE', #10026 ) ;
#18677 = ORIENTED_EDGE ( 'NONE', *, *, #11519, .T. ) ;
#18678 = CARTESIAN_POINT ( 'NONE',  ( 1.899999999999999023, 0.000000000000000000, -8.239200000000002078 ) ) ;
#18679 = CARTESIAN_POINT ( 'NONE',  ( 0.000000000000000000, 0.000000000000000000, 32.00000000000000000 ) ) ;
#18680 = CARTESIAN_POINT ( 'NONE',  ( -0.7741991708318890497, 4.888101187500000222, -10.96874999795161720 ) ) ;
#18681 = ORIENTED_EDGE ( 'NONE', *, *, #13470, .T. ) ;
#18682 = CARTESIAN_POINT ( 'NONE',  ( 6.234374998975811266, 4.584782303107579615, 2.647025296875021638 ) ) ;
#18683 = CARTESIAN_POINT ( 'NONE',  ( 0.006931111373678406143, -9.685942809247212182, 22.53293026234500473 ) ) ;
#18684 = ORIENTED_EDGE ( 'NONE', *, *, #9100, .F. ) ;
#18685 = CARTESIAN_POINT ( 'NONE',  ( 11.96874999795161365, 3.114526743279308896, -3.846120219227901593 ) ) ;
#18686 = CYLINDRICAL_SURFACE ( 'NONE', #16320, 1.000000000000002442 ) ;
#18687 = EDGE_CURVE ( 'NONE', #14452, #18235, #4200, .T. ) ;
#18688 = FACE_OUTER_BOUND ( 'NONE', #7241, .T. ) ;
#18689 = DIRECTION ( 'NONE',  ( 1.000000000000000000, 0.000000000000000000, 0.000000000000000000 ) ) ;
#18690 = CARTESIAN_POINT ( 'NONE',  ( 0.7741991708318548548, -4.888101187500005551, -10.96874999795161720 ) ) ;
#18691 = EDGE_LOOP ( 'NONE', ( #10478, #3005 ) ) ;
#18692 = AXIS2_PLACEMENT_3D ( 'NONE', #7051, #14782, #7248 ) ;
#18693 = FACE_OUTER_BOUND ( 'NONE', #4782, .T. ) ;
#18694 = DIRECTION ( 'NONE',  ( 1.000000000000000000, 0.000000000000000000, 0.000000000000000000 ) ) ;
#18695 = DIRECTION ( 'NONE',  ( 0.000000000000000000, 0.5877852522924629231, 0.8090169943749548898 ) ) ;
#18696 = VERTEX_POINT ( 'NONE', #3807 ) ;
#18697 = LINE ( 'NONE', #12316, #6612 ) ;
#18698 = CARTESIAN_POINT ( 'NONE',  ( 14.00000000000000178, 1.714505518806294835E-15, 32.00000000000000000 ) ) ;
#18699 = CARTESIAN_POINT ( 'NONE',  ( -19.00000000000000355, -3.278623949159157558, -2.625000000000002220 ) ) ;
#18700 = CARTESIAN_POINT ( 'NONE',  ( 7.671566133830872047, 15.77352024078954784, -32.00000000000000000 ) ) ;
#18701 = ORIENTED_EDGE ( 'NONE', *, *, #15251, .T. ) ;
#18702 = CARTESIAN_POINT ( 'NONE',  ( 12.32184790671639618, 13.12143529358541016, 32.00000000000000000 ) ) ;
#18703 = DIRECTION ( 'NONE',  ( 1.000000000000000000, 0.000000000000000000, 0.000000000000000000 ) ) ;
#18704 = EDGE_LOOP ( 'NONE', ( #14927, #12126 ) ) ;
#18705 = CARTESIAN_POINT ( 'NONE',  ( 8.468749997951615427, -2.873153789725853002, 3.954556930911842016 ) ) ;
#18706 = EDGE_CURVE ( 'NONE', #15548, #3069, #9987, .T. ) ;
#18707 = CARTESIAN_POINT ( 'NONE',  ( 0.7592463834391192101, -12.05220173035421993, -24.80264696524895385 ) ) ;
#18708 = EDGE_CURVE ( 'NONE', #9066, #1328, #2623, .T. ) ;
#18709 = AXIS2_PLACEMENT_3D ( 'NONE', #4436, #5631, #13254 ) ;
#18710 = ORIENTED_EDGE ( 'NONE', *, *, #93, .T. ) ;
#18711 = B_SPLINE_CURVE_WITH_KNOTS ( 'NONE', 3,
 ( #7858, #671, #2161, #9683, #15775, #14170 ),
 .UNSPECIFIED., .F., .F.,
 ( 4, 2, 4 ),
 ( 4.462636677693390501E-07, 0.001879885020955133004, 0.003759323778242496666 ),
 .UNSPECIFIED. ) ;
#18712 = ADVANCED_FACE ( 'NONE', ( #2400 ), #14620, .F. ) ;
#18713 = CARTESIAN_POINT ( 'NONE',  ( -15.00000000000000355, 1.224646799147353454E-16, 0.000000000000000000 ) ) ;
#18714 = DIRECTION ( 'NONE',  ( 0.000000000000000000, 0.000000000000000000, -1.000000000000000000 ) ) ;
#18715 = EDGE_CURVE ( 'NONE', #15581, #10033, #9020, .T. ) ;
#18716 = ORIENTED_EDGE ( 'NONE', *, *, #10080, .F. ) ;
#18717 = CARTESIAN_POINT ( 'NONE',  ( 0.000000000000000000, 9.324097380959415204, 22.25075486061743391 ) ) ;
#18718 = CARTESIAN_POINT ( 'NONE',  ( 1.039999999999995373, -12.96210679857767900, -24.89775460606846380 ) ) ;
#18719 = VERTEX_POINT ( 'NONE', #12005 ) ;
#18720 = DIRECTION ( 'NONE',  ( -1.000000000000000000, -0.000000000000000000, -0.000000000000000000 ) ) ;
#18721 = VERTEX_POINT ( 'NONE', #16411 ) ;
#18722 = CARTESIAN_POINT ( 'NONE',  ( 2.299999999999998934, 0.000000000000000000, -6.200000000000021494 ) ) ;
#18723 = TOROIDAL_SURFACE ( 'NONE', #4032, 4.200000000000000178, 0.1999999999999998723 ) ;
#18724 = VERTEX_POINT ( 'NONE', #18108 ) ;
#18725 = DIRECTION ( 'NONE',  ( 1.000000000000000000, 0.000000000000000000, 0.000000000000000000 ) ) ;
#18726 = TOROIDAL_SURFACE ( 'NONE', #13298, 8.800000000000023803, 0.1999999999999994282 ) ;
#18727 = CARTESIAN_POINT ( 'NONE',  ( 1.016293382781377819, -4.781284448697200595, -7.843749997951614539 ) ) ;
#18728 = EDGE_CURVE ( 'NONE', #11304, #3344, #16053, .T. ) ;
#18729 = DIRECTION ( 'NONE',  ( -1.000000000000000000, -0.000000000000000000, 0.000000000000000000 ) ) ;
#18730 = CARTESIAN_POINT ( 'NONE',  ( 9.580134541264516912, -14.56230589874905412, -32.00000000000000000 ) ) ;
#18731 = VERTEX_POINT ( 'NONE', #13700 ) ;
#18732 = DIRECTION ( 'NONE',  ( 0.000000000000000000, 0.000000000000000000, 1.000000000000000000 ) ) ;
#18733 = LINE ( 'NONE', #5121, #1469 ) ;
#18734 = EDGE_LOOP ( 'NONE', ( #19211, #6927, #7122, #14073 ) ) ;
#18735 = EDGE_CURVE ( 'NONE', #16271, #155, #10508, .T. ) ;
#18736 = CIRCLE ( 'NONE', #14273, 2.524999999999995914 ) ;
#18737 = LINE ( 'NONE', #17241, #15444 ) ;
#18738 = AXIS2_PLACEMENT_3D ( 'NONE', #15302, #13491, #2880 ) ;
#18739 = EDGE_CURVE ( 'NONE', #3268, #14183, #428, .T. ) ;
#18740 = CARTESIAN_POINT ( 'NONE',  ( 14.86923836996420434, -11.47363181547641453, -32.00000000000000000 ) ) ;
#18741 = DIRECTION ( 'NONE',  ( -1.000000000000000000, 1.224646799147353207E-16, 0.000000000000000000 ) ) ;
#18742 = EDGE_CURVE ( 'NONE', #7627, #6438, #15308, .T. ) ;
#18743 = ORIENTED_EDGE ( 'NONE', *, *, #8191, .T. ) ;
#18744 = CARTESIAN_POINT ( 'NONE',  ( 10.00000000000000533, -4.235925505221111997, -3.814044456245531567 ) ) ;
#18745 = LINE ( 'NONE', #5039, #4334 ) ;
#18746 = VERTEX_POINT ( 'NONE', #9204 ) ;
#18747 = FACE_BOUND ( 'NONE', #4000, .T. ) ;
#18748 = VERTEX_POINT ( 'NONE', #2686 ) ;
#18749 = APPLICATION_PROTOCOL_DEFINITION ( 'draft international standard', 'automotive_design', 1998, #15199 ) ;
#18750 = CARTESIAN_POINT ( 'NONE',  ( -5.574407415329146964, 1.493657965219562067, -13.50000000000000533 ) ) ;
#18751 = SURFACE_STYLE_FILL_AREA ( #6532 ) ;
#18752 = EDGE_CURVE ( 'NONE', #2248, #9739, #15208, .T. ) ;
#18753 = ORIENTED_EDGE ( 'NONE', *, *, #12718, .T. ) ;
#18754 = ORIENTED_EDGE ( 'NONE', *, *, #17881, .T. ) ;
#18755 = CARTESIAN_POINT ( 'NONE',  ( 0.3599332783571699279, -23.15620303736534069, 12.90954937922492007 ) ) ;
#18756 = VECTOR ( 'NONE', #10585, 1000.000000000000114 ) ;
#18757 = LINE ( 'NONE', #17069, #11749 ) ;
#18758 = ORIENTED_EDGE ( 'NONE', *, *, #19473, .T. ) ;
#18759 = EDGE_CURVE ( 'NONE', #1519, #17434, #15201, .T. ) ;
#18760 = EDGE_CURVE ( 'NONE', #4468, #1215, #17116, .T. ) ;
#18761 = CARTESIAN_POINT ( 'NONE',  ( 2.718184767880468478, 23.19431517146933430, 10.24584646439546987 ) ) ;
#18762 = EDGE_LOOP ( 'NONE', ( #1543, #16776 ) ) ;
#18763 = AXIS2_PLACEMENT_3D ( 'NONE', #5216, #11335, #14721 ) ;
#18764 = CARTESIAN_POINT ( 'NONE',  ( -25.31088913245573835, 82.80384757729319745, 37.99999999999999289 ) ) ;
#18765 = CIRCLE ( 'NONE', #17490, 2.524999999999995914 ) ;
#18766 = DIRECTION ( 'NONE',  ( 0.000000000000000000, 0.000000000000000000, 1.000000000000000000 ) ) ;
#18767 = FACE_OUTER_BOUND ( 'NONE', #7506, .T. ) ;
#18768 = EDGE_LOOP ( 'NONE', ( #16485, #17307, #11426, #14230 ) ) ;
#18769 = CARTESIAN_POINT ( 'NONE',  ( 4.762500000000000178, 5.832380380939270108E-16, -6.502399999999998847 ) ) ;
#18770 = PRESENTATION_STYLE_ASSIGNMENT (( #16590 ) ) ;
#18771 = EDGE_CURVE ( 'NONE', #18915, #7834, #1347, .T. ) ;
#18772 = EDGE_LOOP ( 'NONE', ( #12865, #11737, #7995, #4128 ) ) ;
#18773 = VERTEX_POINT ( 'NONE', #6181 ) ;
#18774 = CARTESIAN_POINT ( 'NONE',  ( -4.235925505221191933, -3.814044456245443193, -7.000000000000005329 ) ) ;
#18775 = CARTESIAN_POINT ( 'NONE',  ( 12.99999999999999467, 4.021726346896418391, -2.778353902928511587 ) ) ;
#18776 = CONICAL_SURFACE ( 'NONE', #9525, 3.593999999999999861, 0.2132412839022293782 ) ;
#18777 = EDGE_CURVE ( 'NONE', #16782, #18923, #17049, .T. ) ;
#18778 = CARTESIAN_POINT ( 'NONE',  ( 0.7741991708318884946, 4.888101187500000222, -11.96874999795161365 ) ) ;
#18779 = EDGE_CURVE ( 'NONE', #10514, #14373, #15106, .T. ) ;
#18780 = CIRCLE ( 'NONE', #11757, 2.524999999999996803 ) ;
#18781 = EDGE_LOOP ( 'NONE', ( #6574, #828, #18230, #15030 ) ) ;
#18782 = CARTESIAN_POINT ( 'NONE',  ( 10.34374999795161543, 0.2590123213421660631, -4.942249507334553371 ) ) ;
#18783 = CARTESIAN_POINT ( 'NONE',  ( -2.000000000000001776, 0.000000000000000000, 0.000000000000000000 ) ) ;
#18784 = ORIENTED_EDGE ( 'NONE', *, *, #17761, .T. ) ;
#18785 = DIRECTION ( 'NONE',  ( 0.000000000000000000, 0.000000000000000000, 1.000000000000000000 ) ) ;
#18786 =( BOUNDED_SURFACE ( )  B_SPLINE_SURFACE ( 1, 2, ( 
 ( #10277, #15070, #10671, #12370, #18175, #12072, #256, #18369, #2853, #15167, #3053, #7442, #7848, #1759, #4856, #16778, #7546 ),
 ( #12268, #16575, #15470, #4660, #13566, #4754, #9168, #6338, #15274, #16971, #13964, #10571, #18462, #3253, #12463, #13867, #159 ) ),
 .UNSPECIFIED., .F., .F., .F. ) 
 B_SPLINE_SURFACE_WITH_KNOTS ( ( 2, 2 ),
 ( 3, 2, 2, 2, 2, 2, 2, 2, 3 ),
 ( 0.000000000000000000, 1.000000000000000000 ),
 ( 0.000000000000000000, 0.05000000000000000278, 0.1000000000000000056, 0.1499999999999999944, 0.2000000000000000111, 0.2500000000000000000, 0.2999999999999999889, 0.3499999999999999778, 0.4000000000000000222 ),
 .UNSPECIFIED. ) 
 GEOMETRIC_REPRESENTATION_ITEM ( )  RATIONAL_B_SPLINE_SURFACE ( (
 ( 1.000000000000000000, 0.9876883405951377704, 1.000000000000000000, 0.9876883405951377704, 1.000000000000000000, 0.9876883405951377704, 1.000000000000000000, 0.9876883405951377704, 1.000000000000000000, 0.9876883405951377704, 1.000000000000000000, 0.9876883405951377704, 1.000000000000000000, 0.9876883405951377704, 1.000000000000000000, 0.9876883405951377704, 1.000000000000000000),
 ( 1.000000000000000000, 0.9876883405951377704, 1.000000000000000000, 0.9876883405951377704, 1.000000000000000000, 0.9876883405951377704, 1.000000000000000000, 0.9876883405951377704, 1.000000000000000000, 0.9876883405951377704, 1.000000000000000000, 0.9876883405951377704, 1.000000000000000000, 0.9876883405951377704, 1.000000000000000000, 0.9876883405951377704, 1.000000000000000000) ) ) 
 REPRESENTATION_ITEM ( '' )  SURFACE ( )  );
#18787 = CARTESIAN_POINT ( 'NONE',  ( 12.34374999795161543, -1.773574444220693325, -4.620319390059841602 ) ) ;
#18788 = EDGE_CURVE ( 'NONE', #2678, #2901, #15405, .T. ) ;
#18789 = CARTESIAN_POINT ( 'NONE',  ( -4.235925505221191933, -3.814044456245443193, -8.312499995903225525 ) ) ;
#18790 = DIRECTION ( 'NONE',  ( -0.000000000000000000, -0.000000000000000000, 1.000000000000000000 ) ) ;
#18791 = CARTESIAN_POINT ( 'NONE',  ( 8.843749997951615427, 4.861323657744407001, 0.5109457054261780096 ) ) ;
#18792 = CIRCLE ( 'NONE', #19127, 1.000000000000004441 ) ;
#18793 = DIRECTION ( 'NONE',  ( 1.000000000000000000, -0.000000000000000000, -0.000000000000000000 ) ) ;
#18794 =( NAMED_UNIT ( * ) PLANE_ANGLE_UNIT ( ) SI_UNIT ( $, .RADIAN. ) );
#18795 = CARTESIAN_POINT ( 'NONE',  ( 0.02436607992776325046, 16.37294372382858398, 18.55949924794898465 ) ) ;
#18796 = CARTESIAN_POINT ( 'NONE',  ( 4.484949146646379781, 3.631840208645794821, -11.81249999590322552 ) ) ;
#18797 = EDGE_LOOP ( 'NONE', ( #12682, #1841, #5592, #19154, #8170, #9568, #13953 ) ) ;
#18798 = FACE_OUTER_BOUND ( 'NONE', #14555, .T. ) ;
#18799 = FACE_OUTER_BOUND ( 'NONE', #161, .T. ) ;
#18800 = PRODUCT_DEFINITION_CONTEXT ( 'detailed design', #13915, 'design' ) ;
#18801 = CARTESIAN_POINT ( 'NONE',  ( 7.000000000000005329, 5.575441324182695446, -1.185096637661215091 ) ) ;
#18802 = CARTESIAN_POINT ( 'NONE',  ( 12.99999999999969980, -3.863910152777011664, 3.836387901770588194 ) ) ;
#18803 = CARTESIAN_POINT ( 'NONE',  ( 0.000000000000000000, -22.25075486061732732, -9.324097380959701198 ) ) ;
#18804 = VERTEX_POINT ( 'NONE', #8081 ) ;
#18805 = CARTESIAN_POINT ( 'NONE',  ( 5.700000000000001066, -0.2987243419133421840, -14.14705514798869679 ) ) ;
#18806 = LINE ( 'NONE', #1806, #19096 ) ;
#18807 = EDGE_CURVE ( 'NONE', #8919, #15015, #11549, .T. ) ;
#18808 = ORIENTED_EDGE ( 'NONE', *, *, #4328, .F. ) ;
#18809 = DIRECTION ( 'NONE',  ( 1.000000000000000000, 0.000000000000000000, 0.000000000000000000 ) ) ;
#18810 = CARTESIAN_POINT ( 'NONE',  ( 0.1882238552569854284, -10.68696068830390900, -23.64332819722392287 ) ) ;
#18811 = AXIS2_PLACEMENT_3D ( 'NONE', #15142, #18246, #13639 ) ;
#18812 = ORIENTED_EDGE ( 'NONE', *, *, #6322, .F. ) ;
#18813 = CONTEXT_DEPENDENT_SHAPE_REPRESENTATION ( #14734, #2183 ) ;
#18814 =( GEOMETRIC_REPRESENTATION_CONTEXT ( 3 ) GLOBAL_UNCERTAINTY_ASSIGNED_CONTEXT ( ( #8401 ) ) GLOBAL_UNIT_ASSIGNED_CONTEXT ( ( #14963, #19753, #11961 ) ) REPRESENTATION_CONTEXT ( 'NONE', 'WORKASPACE' ) );
#18815 = CARTESIAN_POINT ( 'NONE',  ( 18.96448111170889206, 1.130229351527639370, -32.00000000000000000 ) ) ;
#18816 = CARTESIAN_POINT ( 'NONE',  ( 1.894165461959355756, 24.59696699259432151, 12.96989951879416303 ) ) ;
#18817 = ORIENTED_EDGE ( 'NONE', *, *, #12251, .F. ) ;
#18818 = CARTESIAN_POINT ( 'NONE',  ( 1.800000000000000488, 0.000000000000000000, 0.000000000000000000 ) ) ;
#18819 = CARTESIAN_POINT ( 'NONE',  ( -0.5958122406255597081, 5.668774803599165857, -15.31249999590322552 ) ) ;
#18820 = CARTESIAN_POINT ( 'NONE',  ( 7.078124996927420476, 0.000000000000000000, -5.294050593750000644 ) ) ;
#18821 = EDGE_CURVE ( 'NONE', #3249, #1207, #10623, .T. ) ;
#18822 = ORIENTED_EDGE ( 'NONE', *, *, #4637, .F. ) ;
#18823 = EDGE_CURVE ( 'NONE', #6659, #17967, #15795, .T. ) ;
#18824 = CARTESIAN_POINT ( 'NONE',  ( 8.468749997951615427, -2.873153789725853002, 3.954556930911842016 ) ) ;
#18825 = ORIENTED_EDGE ( 'NONE', *, *, #1148, .F. ) ;
#18827 = LINE ( 'NONE', #15634, #19403 ) ;
#18826 = VECTOR ( 'NONE', #4645, 1000.000000000000000 ) ;
#18828 = EDGE_LOOP ( 'NONE', ( #12453, #5136, #13406, #7972 ) ) ;
#18829 = DIRECTION ( 'NONE',  ( -1.000000000000000000, -0.000000000000000000, -0.000000000000000000 ) ) ;
#18830 = DIRECTION ( 'NONE',  ( -1.000000000000000000, 0.000000000000000000, 0.000000000000000000 ) ) ;
#18831 = CARTESIAN_POINT ( 'NONE',  ( -2.255998204157477538, -17.85806462366060288, 32.00000000000000000 ) ) ;
#18832 = AXIS2_PLACEMENT_3D ( 'NONE', #14561, #12957, #13053 ) ;
#18833 = DIRECTION ( 'NONE',  ( 1.000000000000000000, 0.000000000000000000, 0.000000000000000000 ) ) ;
#18834 = ADVANCED_FACE ( 'NONE', ( #18688 ), #6370, .F. ) ;
#18835 = EDGE_CURVE ( 'NONE', #15601, #8963, #1789, .T. ) ;
#18836 = ORIENTED_EDGE ( 'NONE', *, *, #333, .T. ) ;
#18837 = CARTESIAN_POINT ( 'NONE',  ( 0.006931054464086492187, 24.42321038836783131, 2.248820353273056405 ) ) ;
#18838 = DIRECTION ( 'NONE',  ( -1.000000000000000000, 0.000000000000000000, 0.000000000000000000 ) ) ;
#18839 = ORIENTED_EDGE ( 'NONE', *, *, #11619, .T. ) ;
#18840 = CYLINDRICAL_SURFACE ( 'NONE', #3277, 13.19999999999999574 ) ;
#18841 = DIRECTION ( 'NONE',  ( 1.000000000000000000, 0.000000000000000000, 0.000000000000000000 ) ) ;
#18842 = CARTESIAN_POINT ( 'NONE',  ( -4.861323657744403448, 0.5109457054262118714, -13.46874999795161543 ) ) ;
#18843 = ORIENTED_EDGE ( 'NONE', *, *, #167, .T. ) ;
#18845 = DIRECTION ( 'NONE',  ( -0.000000000000000000, -0.000000000000000000, 1.000000000000000000 ) ) ;
#18844 = AXIS2_PLACEMENT_3D ( 'NONE', #13311, #943, #1511 ) ;
#18846 = CARTESIAN_POINT ( 'NONE',  ( 11.34374999795161543, 1.773574444220790136, -4.620319390059805187 ) ) ;
#18847 = CARTESIAN_POINT ( 'NONE',  ( 13.00000000000000178, -0.6516788101670404343, -4.844895625238700987 ) ) ;
#18848 = EDGE_LOOP ( 'NONE', ( #5412, #16967, #14499, #16373 ) ) ;
#18849 = LINE ( 'NONE', #1939, #14527 ) ;
#18850 = ORIENTED_EDGE ( 'NONE', *, *, #6032, .T. ) ;
#18851 = ITEM_DEFINED_TRANSFORMATION ( 'NONE', 'NONE', #616,  #16724 ) ;
#18852 = FILL_AREA_STYLE_COLOUR ( '', #17669 ) ;
#18853 = CARTESIAN_POINT ( 'NONE',  ( 9.468749997951615427, 4.465502636338023912, 1.988169868018593300 ) ) ;
#18854 = EDGE_LOOP ( 'NONE', ( #5273, #3269, #10413, #3091 ) ) ;
#18855 = ORIENTED_EDGE ( 'NONE', *, *, #15007, .F. ) ;
#18856 = CARTESIAN_POINT ( 'NONE',  ( -8.051804217113518143E-16, 5.456805104201102985, 23.69843731927169728 ) ) ;
#18857 = CARTESIAN_POINT ( 'NONE',  ( 7.000000000000005329, 3.814044456245473835, 4.235925505221166176 ) ) ;
#18858 = FACE_BOUND ( 'NONE', #11796, .T. ) ;
#18859 = ORIENTED_EDGE ( 'NONE', *, *, #17661, .T. ) ;
#18860 = EDGE_CURVE ( 'NONE', #1752, #2115, #4542, .T. ) ;
#18861 = ADVANCED_FACE ( 'NONE', ( #7981 ), #10995, .F. ) ;
#18862 = TOROIDAL_SURFACE ( 'NONE', #10875, 24.12539914357697768, 8.000000000000000000 ) ;
#18863 = VECTOR ( 'NONE', #8837, 1000.000000000000000 ) ;
#18864 = CARTESIAN_POINT ( 'NONE',  ( 1.039999999999996927, 20.02152543075374069, -19.67366047555508501 ) ) ;
#18865 = VERTEX_POINT ( 'NONE', #14088 ) ;
#18866 = ADVANCED_FACE ( 'NONE', ( #18889 ), #17195, .T. ) ;
#18867 = CYLINDRICAL_SURFACE ( 'NONE', #10845, 4.000000000000000000 ) ;
#18868 = CARTESIAN_POINT ( 'NONE',  ( 0.000000000000000000, 0.000000000000000000, 0.000000000000000000 ) ) ;
#18869 = FACE_BOUND ( 'NONE', #16567, .T. ) ;
#18870 = ADVANCED_FACE ( 'NONE', ( #14191 ), #6567, .T. ) ;
#18871 = ORIENTED_EDGE ( 'NONE', *, *, #5392, .F. ) ;
#18872 = LINE ( 'NONE', #7211, #7231 ) ;
#18873 = SURFACE_STYLE_USAGE ( .BOTH. , #5157 ) ;
#18874 = EDGE_CURVE ( 'NONE', #8156, #4149, #6464, .T. ) ;
#18875 = STYLED_ITEM ( 'NONE', ( #4993 ), #15876 ) ;
#18876 =( NAMED_UNIT ( * ) SI_UNIT ( $, .STERADIAN. ) SOLID_ANGLE_UNIT ( ) );
#18877 = ORIENTED_EDGE ( 'NONE', *, *, #13795, .T. ) ;
#18878 = ORIENTED_EDGE ( 'NONE', *, *, #2688, .F. ) ;
#18879 = CARTESIAN_POINT ( 'NONE',  ( -1.280903732194386802, 4.780397808154273065, -13.96874999795161365 ) ) ;
#18880 = CARTESIAN_POINT ( 'NONE',  ( 13.00000000000000178, 3.869963285057293145, -2.986818217332015024 ) ) ;
#18881 = CARTESIAN_POINT ( 'NONE',  ( -7.937500000000000000, -4.582717761692664205, -0.7089489049740167470 ) ) ;
#18882 = EDGE_LOOP ( 'NONE', ( #14622, #10638 ) ) ;
#18883 = CARTESIAN_POINT ( 'NONE',  ( -13.86923836996420967, -11.47363181547641275, 32.00000000000000000 ) ) ;
#18884 = CARTESIAN_POINT ( 'NONE',  ( 6.234374998975811266, 4.584782303107598267, -2.647025296874989664 ) ) ;
#18885 = CIRCLE ( 'NONE', #5465, 6.000000000000000000 ) ;
#18886 = ORIENTED_EDGE ( 'NONE', *, *, #124, .F. ) ;
#18887 = CARTESIAN_POINT ( 'NONE',  ( -7.937500000000000000, -4.582717761692662428, -6.527800000000000047 ) ) ;
#18888 = CARTESIAN_POINT ( 'NONE',  ( 11.50000000000000355, 5.700000000000000178, 0.9027913098498565603 ) ) ;
#18889 = FACE_OUTER_BOUND ( 'NONE', #1058, .T. ) ;
#18890 = CARTESIAN_POINT ( 'NONE',  ( -2.000000000000001776, 0.000000000000000000, 0.000000000000000000 ) ) ;
#18891 = DIRECTION ( 'NONE',  ( -0.000000000000000000, -0.000000000000000000, 1.000000000000000000 ) ) ;
#18892 = DIRECTION ( 'NONE',  ( 0.000000000000000000, 0.000000000000000000, 1.000000000000000000 ) ) ;
#18893 =( LENGTH_UNIT ( ) NAMED_UNIT ( * ) SI_UNIT ( .MILLI., .METRE. ) );
#18894 = DIRECTION ( 'NONE',  ( 1.000000000000000000, 0.000000000000000000, 0.000000000000000000 ) ) ;
#18895 = ORIENTED_EDGE ( 'NONE', *, *, #13204, .F. ) ;
#18896 = CARTESIAN_POINT ( 'NONE',  ( 22.00000000000000355, 2.694222958124177204E-15, -32.00000000000000000 ) ) ;
#18897 = CIRCLE ( 'NONE', #14441, 1.000000000000002665 ) ;
#18898 = SURFACE_STYLE_FILL_AREA ( #12801 ) ;
#18899 = CARTESIAN_POINT ( 'NONE',  ( 5.574407415329170057, 1.493657965219485018, -9.812499995903223748 ) ) ;
#18900 = CIRCLE ( 'NONE', #2278, 4.200000000000000178 ) ;
#18901 = CARTESIAN_POINT ( 'NONE',  ( 8.000000000000005329, 2.318398865532038666, 5.207209108562838473 ) ) ;
#18902 = CARTESIAN_POINT ( 'NONE',  ( 14.34374999795161365, 1.280903732194486722, -4.780397808154247308 ) ) ;
#18903 = EDGE_LOOP ( 'NONE', ( #4887, #4938, #12136, #15067, #1299, #9919 ) ) ;
#18904 = DIRECTION ( 'NONE',  ( -1.000000000000000000, -0.000000000000000000, 0.000000000000000000 ) ) ;
#18905 = ORIENTED_EDGE ( 'NONE', *, *, #174, .T. ) ;
#18906 = CARTESIAN_POINT ( 'NONE',  ( 2.000000000000001776, 0.000000000000000000, 0.000000000000000000 ) ) ;
#18907 = CARTESIAN_POINT ( 'NONE',  ( -14.19790265903626647, 9.644882309621941374, -32.00000000000000000 ) ) ;
#18908 = ORIENTED_EDGE ( 'NONE', *, *, #12486, .T. ) ;
#18909 = FILL_AREA_STYLE ('',( #5400 ) ) ;
#18910 = DIRECTION ( 'NONE',  ( 0.000000000000000000, 1.000000000000000000, 0.000000000000000000 ) ) ;
#18911 = AXIS2_PLACEMENT_3D ( 'NONE', #1297, #7582, #2991 ) ;
#18912 = VECTOR ( 'NONE', #7148, 1000.000000000000000 ) ;
#18913 = LINE ( 'NONE', #9527, #1649 ) ;
#18914 = DIRECTION ( 'NONE',  ( 0.000000000000000000, 0.000000000000000000, 1.000000000000000000 ) ) ;
#18915 = VERTEX_POINT ( 'NONE', #10798 ) ;
#18916 = B_SPLINE_CURVE_WITH_KNOTS ( 'NONE', 3,
 ( #15096, #4481, #4585, #7672 ),
 .UNSPECIFIED., .F., .F.,
 ( 4, 4 ),
 ( 2.034713381942770827E-07, 0.0006887909409525120848 ),
 .UNSPECIFIED. ) ;
#18917 = DIRECTION ( 'NONE',  ( 1.000000000000000000, 0.000000000000000000, 0.000000000000000000 ) ) ;
#18918 = CARTESIAN_POINT ( 'NONE',  ( -15.00000000000000355, 1.224646799147353454E-16, 0.000000000000000000 ) ) ;
#18919 = ADVANCED_FACE ( 'NONE', ( #3188 ), #9299, .T. ) ;
#18920 = CIRCLE ( 'NONE', #11582, 5.700000000000001954 ) ;
#18921 = EDGE_LOOP ( 'NONE', ( #17863, #5369 ) ) ;
#18922 = FACE_OUTER_BOUND ( 'NONE', #14542, .T. ) ;
#18923 = VERTEX_POINT ( 'NONE', #12601 ) ;
#18924 = CARTESIAN_POINT ( 'NONE',  ( 17.68117051311639898, -3.372863662543048591, 35.00000000000000000 ) ) ;
#18925 = ORIENTED_EDGE ( 'NONE', *, *, #7632, .F. ) ;
#18926 = CARTESIAN_POINT ( 'NONE',  ( 1.749999999999998002, 4.147968289691286614, 27.76164181293053090 ) ) ;
#18927 = CARTESIAN_POINT ( 'NONE',  ( 8.671566133830875600, 15.77352024078954784, 32.00000000000000000 ) ) ;
#18928 = FACE_OUTER_BOUND ( 'NONE', #13257, .T. ) ;
#18929 = VECTOR ( 'NONE', #12403, 1000.000000000000114 ) ;
#18930 = STYLED_ITEM ( 'NONE', ( #11262 ), #9200 ) ;
#18931 = DIRECTION ( 'NONE',  ( -1.000000000000000000, -0.000000000000000000, -0.000000000000000000 ) ) ;
#18932 = ORIENTED_EDGE ( 'NONE', *, *, #6801, .F. ) ;
#18933 = PLANE ( 'NONE',  #3874 ) ;
#18934 = DIRECTION ( 'NONE',  ( 0.000000000000000000, 0.000000000000000000, 1.000000000000000000 ) ) ;
#18935 = VERTEX_POINT ( 'NONE', #2080 ) ;
#18936 = MECHANICAL_DESIGN_GEOMETRIC_PRESENTATION_REPRESENTATION (  '', ( #414 ), #2964 ) ;
#18937 = EDGE_CURVE ( 'NONE', #4963, #4614, #15693, .T. ) ;
#18938 = PLANE ( 'NONE',  #5828 ) ;
#18939 =( REPRESENTATION_RELATIONSHIP ('NONE','NONE', #18211, #19604 ) REPRESENTATION_RELATIONSHIP_WITH_TRANSFORMATION ( #11017 )SHAPE_REPRESENTATION_RELATIONSHIP( ) );
#18940 = LINE ( 'NONE', #8027, #8354 ) ;
#18941 = CARTESIAN_POINT ( 'NONE',  ( 0.000000000000000000, 0.000000000000000000, -6.502399999999998847 ) ) ;
#18942 = ORIENTED_EDGE ( 'NONE', *, *, #11013, .F. ) ;
#18943 = TOROIDAL_SURFACE ( 'NONE', #8067, 7.800000000000000711, 0.1999999999999998723 ) ;
#18944 = DIRECTION ( 'NONE',  ( 1.000000000000000000, 0.000000000000000000, 0.000000000000000000 ) ) ;
#18945 = CARTESIAN_POINT ( 'NONE',  ( 4.080749450109622423, -4.080749450109678378, -8.500000000000005329 ) ) ;
#18946 = CARTESIAN_POINT ( 'NONE',  ( -17.11901729331276911, 5.562305898749051458, -32.00000000000000000 ) ) ;
#18947 = ADVANCED_FACE ( 'NONE', ( #18495 ), #18290, .T. ) ;
#18948 = ORIENTED_EDGE ( 'NONE', *, *, #8569, .T. ) ;
#18949 = DIRECTION ( 'NONE',  ( 1.000000000000000000, 0.000000000000000000, 0.000000000000000000 ) ) ;
#18950 = EDGE_LOOP ( 'NONE', ( #4643, #14299, #9466, #17480, #10091 ) ) ;
#18951 = CONTEXT_DEPENDENT_SHAPE_REPRESENTATION ( #10650, #3955 ) ;
#18952 = CARTESIAN_POINT ( 'NONE',  ( 12.34374999795161543, -3.114526743279282250, 3.846120219227923798 ) ) ;
#18953 = VECTOR ( 'NONE', #13249, 1000.000000000000000 ) ;
#18954 = EDGE_LOOP ( 'NONE', ( #13592, #7511, #7101, #3547 ) ) ;
#18955 = ORIENTED_EDGE ( 'NONE', *, *, #4214, .T. ) ;
#18956 = CARTESIAN_POINT ( 'NONE',  ( 4.409619785863891472, -2.246813503491864150, -8.343749997951611874 ) ) ;
#18957 = CARTESIAN_POINT ( 'NONE',  ( 8.312499995903225525, -1.761396867937238486, 5.421022142882364392 ) ) ;
#18958 = CARTESIAN_POINT ( 'NONE',  ( 8.000000000000000000, 0.000000000000000000, 0.000000000000000000 ) ) ;
#18959 = ORIENTED_EDGE ( 'NONE', *, *, #4591, .T. ) ;
#18960 = COLOUR_RGB ( '', 0.40784314, 0.44705882, 0.49803922) ;
#18961 = CARTESIAN_POINT ( 'NONE',  ( 2.257825491203654611, 24.44564404695844573, 11.58891744060115947 ) ) ;
#18962 = EDGE_CURVE ( 'NONE', #18640, #9108, #13818, .T. ) ;
#18963 = ORIENTED_EDGE ( 'NONE', *, *, #18742, .T. ) ;
#18964 = AXIS2_PLACEMENT_3D ( 'NONE', #12695, #10897, #9707 ) ;
#18965 = ADVANCED_FACE ( 'NONE', ( #6963, #2377 ), #17492, .F. ) ;
#18966 = DIRECTION ( 'NONE',  ( 0.000000000000000000, -0.8660254037844363761, -0.5000000000000039968 ) ) ;
#18967 = CARTESIAN_POINT ( 'NONE',  ( 7.500000000000005329, -2.620002426024580000, 5.142044285764733935 ) ) ;
#18968 = CARTESIAN_POINT ( 'NONE',  ( -4.781284448697179279, 1.016293382781477961, -10.46874999795161720 ) ) ;
#18969 = EDGE_CURVE ( 'NONE', #6839, #10551, #17687, .T. ) ;
#18970 = VERTEX_POINT ( 'NONE', #17589 ) ;
#18971 = DIRECTION ( 'NONE',  ( -0.000000000000000000, -0.000000000000000000, 1.000000000000000000 ) ) ;
#18972 = SURFACE_STYLE_FILL_AREA ( #1060 ) ;
#18973 = CARTESIAN_POINT ( 'NONE',  ( 13.00000000000000000, -4.333424887442987483, -2.261628166637620119 ) ) ;
#18974 = EDGE_LOOP ( 'NONE', ( #1867, #3759, #19528, #16512 ) ) ;
#18975 = ORIENTED_EDGE ( 'NONE', *, *, #1342, .T. ) ;
#18976 = LINE ( 'NONE', #2269, #5056 ) ;
#18977 = VECTOR ( 'NONE', #9232, 1000.000000000000000 ) ;
#18978 = EDGE_CURVE ( 'NONE', #5549, #8517, #6758, .T. ) ;
#18979 = DIRECTION ( 'NONE',  ( -1.000000000000000000, -0.000000000000000000, 0.000000000000000000 ) ) ;
#18980 = CARTESIAN_POINT ( 'NONE',  ( 0.02436607992776238310, -12.59161484032927092, 21.30679549418627161 ) ) ;
#18981 = ORIENTED_EDGE ( 'NONE', *, *, #17144, .F. ) ;
#18982 = CARTESIAN_POINT ( 'NONE',  ( 9.968749997951617203, 0.2590123213421660631, -4.942249507334553371 ) ) ;
#18983 = CARTESIAN_POINT ( 'NONE',  ( 12.92161831991541554, 3.713244971082770629, -3.181176262573004898 ) ) ;
#18984 = AXIS2_PLACEMENT_3D ( 'NONE', #2845, #1355, #7434 ) ;
#18985 = ORIENTED_EDGE ( 'NONE', *, *, #5857, .T. ) ;
#18986 = DIRECTION ( 'NONE',  ( 0.000000000000000000, 0.000000000000000000, -1.000000000000000000 ) ) ;
#18987 = EDGE_CURVE ( 'NONE', #12173, #3750, #12120, .T. ) ;
#18988 = EDGE_CURVE ( 'NONE', #15386, #750, #17335, .T. ) ;
#18989 = CARTESIAN_POINT ( 'NONE',  ( 9.500000000000005329, 5.142044285764750811, -2.620002426024544473 ) ) ;
#18990 = AXIS2_PLACEMENT_3D ( 'NONE', #10608, #16610, #4304 ) ;
#18991 = CARTESIAN_POINT ( 'NONE',  ( 0.07186811453410632544, -18.89333555428542155, -16.91241718342019951 ) ) ;
#18992 = DIRECTION ( 'NONE',  ( 1.000000000000000000, 0.000000000000000000, 0.000000000000000000 ) ) ;
#18993 = CARTESIAN_POINT ( 'NONE',  ( -2.246813503491864150, -4.409619785863891472, -12.96874999795161543 ) ) ;
#18994 = LINE ( 'NONE', #8393, #18425 ) ;
#18995 = SHAPE_REPRESENTATION_RELATIONSHIP ( 'NONE' , 'NONE' ,  #7967, #5887 ) ;
#18996 = DIRECTION ( 'NONE',  ( 0.000000000000000000, 0.000000000000000000, 1.000000000000000000 ) ) ;
#18997 = CARTESIAN_POINT ( 'NONE',  ( 5.700000000000001066, 0.5990941410143484358, -13.64430100820693603 ) ) ;
#18998 = ORIENTED_EDGE ( 'NONE', *, *, #15621, .T. ) ;
#18999 = CARTESIAN_POINT ( 'NONE',  ( -10.58013454126452224, -14.56230589874905235, 32.00000000000000000 ) ) ;
#19000 = VECTOR ( 'NONE', #16756, 1000.000000000000000 ) ;
#19001 = DIRECTION ( 'NONE',  ( 0.000000000000000000, 0.000000000000000000, 1.000000000000000000 ) ) ;
#19002 = UNCERTAINTY_MEASURE_WITH_UNIT (LENGTH_MEASURE( 1.000000000000000082E-05 ), #13091, 'distance_accuracy_value', 'NONE');
#19003 = CARTESIAN_POINT ( 'NONE',  ( 2.789999999999999147, -18.55949924794904504, 16.37294372382852004 ) ) ;
#19004 = EDGE_CURVE ( 'NONE', #12710, #4605, #11488, .T. ) ;
#19005 = CARTESIAN_POINT ( 'NONE',  ( 6.843749997951615427, -4.233219804643904460, 2.444050593749960587 ) ) ;
#19006 = DIRECTION ( 'NONE',  ( 0.1045284632676418274, -0.9945218953682745111, 0.000000000000000000 ) ) ;
#19007 = CARTESIAN_POINT ( 'NONE',  ( -5.142044285764750811, 2.620002426024544029, -8.812499995903225525 ) ) ;
#19008 = ORIENTED_EDGE ( 'NONE', *, *, #504, .F. ) ;
#19009 = AXIS2_PLACEMENT_3D ( 'NONE', #1407, #7488, #9409 ) ;
#19010 = FACE_OUTER_BOUND ( 'NONE', #6931, .T. ) ;
#19011 = FACE_OUTER_BOUND ( 'NONE', #17676, .T. ) ;
#19012 = EDGE_CURVE ( 'NONE', #19760, #18970, #16196, .T. ) ;
#19013 = ORIENTED_EDGE ( 'NONE', *, *, #4824, .F. ) ;
#19014 = DIRECTION ( 'NONE',  ( 1.000000000000000000, 6.419766481290786633E-33, -0.000000000000000000 ) ) ;
#19015 = CIRCLE ( 'NONE', #5271, 0.9999999999999974465 ) ;
#19016 = CARTESIAN_POINT ( 'NONE',  ( 6.656249997951614539, 0.000000000000000000, -5.700000000000001066 ) ) ;
#19017 = DIRECTION ( 'NONE',  ( 0.000000000000000000, 0.000000000000000000, 1.000000000000000000 ) ) ;
#19018 = ORIENTED_EDGE ( 'NONE', *, *, #17852, .F. ) ;
#19019 = CARTESIAN_POINT ( 'NONE',  ( -3.000000000000002665, 1.224646799147353256E-15, -10.00000000000000000 ) ) ;
#19020 = CARTESIAN_POINT ( 'NONE',  ( -5.387740456496205255, 2.068159791354258648, -11.81249999590322552 ) ) ;
#19021 = CARTESIAN_POINT ( 'NONE',  ( 3.114526743279282694, 3.846120219227923798, -7.343749997951615427 ) ) ;
#19022 = ORIENTED_EDGE ( 'NONE', *, *, #10725, .F. ) ;
#19023 = CARTESIAN_POINT ( 'NONE',  ( 10.96874999795161720, -4.888101187500005551, 0.7741991708318548548 ) ) ;
#19024 = ORIENTED_EDGE ( 'NONE', *, *, #16974, .F. ) ;
#19025 = CARTESIAN_POINT ( 'NONE',  ( -90.00000000000000000, 0.000000000000000000, -8.265000000000021885 ) ) ;
#19026 = ORIENTED_EDGE ( 'NONE', *, *, #17974, .F. ) ;
#19027 = PLANE ( 'NONE',  #5098 ) ;
#19028 = DIRECTION ( 'NONE',  ( 0.000000000000000000, 0.000000000000000000, 1.000000000000000000 ) ) ;
#19029 = EDGE_CURVE ( 'NONE', #16926, #3728, #17961, .T. ) ;
#19030 = DIRECTION ( 'NONE',  ( -1.000000000000000000, -0.000000000000000000, -0.000000000000000000 ) ) ;
#19031 = AXIS2_PLACEMENT_3D ( 'NONE', #5939, #43, #3041 ) ;
#19032 = CARTESIAN_POINT ( 'NONE',  ( -5.700000000000000178, 0.9027913098498568933, -6.500000000000005329 ) ) ;
#19033 = AXIS2_PLACEMENT_3D ( 'NONE', #17484, #13078, #14386 ) ;
#19034 = ORIENTED_EDGE ( 'NONE', *, *, #8634, .F. ) ;
#19035 = FACE_BOUND ( 'NONE', #13246, .T. ) ;
#19036 = DIRECTION ( 'NONE',  ( -1.000000000000000000, 0.000000000000000000, 0.000000000000000000 ) ) ;
#19037 = VERTEX_POINT ( 'NONE', #5569 ) ;
#19038 = EDGE_CURVE ( 'NONE', #10239, #8854, #11678, .T. ) ;
#19039 = DIRECTION ( 'NONE',  ( 0.000000000000000000, 0.000000000000000000, -1.000000000000000000 ) ) ;
#19040 = CARTESIAN_POINT ( 'NONE',  ( 3.292592168578600820, 7.264456548524799828, 4.858580985450665956E-15 ) ) ;
#19041 = CARTESIAN_POINT ( 'NONE',  ( 0.7592463896980138349, 19.86438386685688684, -19.12676442129323107 ) ) ;
#19042 = ORIENTED_EDGE ( 'NONE', *, *, #3919, .F. ) ;
#19043 = CARTESIAN_POINT ( 'NONE',  ( -7.671566133830872047, 15.77352024078954429, -35.00000000000000000 ) ) ;
#19044 = EDGE_CURVE ( 'NONE', #19760, #18565, #715, .T. ) ;
#19045 = CARTESIAN_POINT ( 'NONE',  ( 0.7741991708318548548, -4.888101187500005551, -10.96874999795161720 ) ) ;
#19046 = DIRECTION ( 'NONE',  ( 0.000000000000000000, 1.776356839400250465E-15, 1.000000000000000000 ) ) ;
#19047 = EDGE_LOOP ( 'NONE', ( #4928, #15242, #19634, #10047 ) ) ;
#19048 = DIRECTION ( 'NONE',  ( 0.000000000000000000, 0.000000000000000000, 1.000000000000000000 ) ) ;
#19049 = ORIENTED_EDGE ( 'NONE', *, *, #5386, .F. ) ;
#19050 = CARTESIAN_POINT ( 'NONE',  ( 12.99999999999969624, -5.254364458093111701, -1.428050399360220490 ) ) ;
#19051 =( LENGTH_UNIT ( ) NAMED_UNIT ( * ) SI_UNIT ( .MILLI., .METRE. ) );
#19052 = LINE ( 'NONE', #10061, #16352 ) ;
#19053 = ORIENTED_EDGE ( 'NONE', *, *, #93, .F. ) ;
#19054 = VERTEX_POINT ( 'NONE', #8676 ) ;
#19055 = CARTESIAN_POINT ( 'NONE',  ( 3.954556930911842016, -2.873153789725853002, -8.843749997951615427 ) ) ;
#19056 = DIRECTION ( 'NONE',  ( -0.000000000000000000, -0.000000000000000000, 1.000000000000000000 ) ) ;
#19057 = FACE_OUTER_BOUND ( 'NONE', #5801, .T. ) ;
#19058 = ORIENTED_EDGE ( 'NONE', *, *, #1740, .F. ) ;
#19059 = ADVANCED_FACE ( 'NONE', ( #9904 ), #14785, .F. ) ;
#19060 = AXIS2_PLACEMENT_3D ( 'NONE', #10308, #13103, #1098 ) ;
#19061 = ORIENTED_EDGE ( 'NONE', *, *, #18008, .T. ) ;
#19062 = CARTESIAN_POINT ( 'NONE',  ( 13.00000000000000533, -0.2990843904630008931, 5.438532396800195734 ) ) ;
#19063 = CARTESIAN_POINT ( 'NONE',  ( 9.500000000000005329, -5.142044285764769462, 2.620002426024508502 ) ) ;
#19064 = EDGE_LOOP ( 'NONE', ( #6533, #5751 ) ) ;
#19065 = CARTESIAN_POINT ( 'NONE',  ( -4.465502636338051445, -1.988169868018530462, -8.468749997951615427 ) ) ;
#19066 = AXIS2_PLACEMENT_3D ( 'NONE', #198, #4897, #10999 ) ;
#19067 = CARTESIAN_POINT ( 'NONE',  ( 4.942249507334556924, 0.2590123213420971182, -12.96874999795161543 ) ) ;
#19068 = CIRCLE ( 'NONE', #15566, 2.524999999999996358 ) ;
#19069 = EDGE_LOOP ( 'NONE', ( #7823, #4635, #5848, #12216 ) ) ;
#19070 = EDGE_CURVE ( 'NONE', #6213, #4951, #12240, .T. ) ;
#19071 = EDGE_CURVE ( 'NONE', #6388, #3148, #11586, .T. ) ;
#19072 = VERTEX_POINT ( 'NONE', #2281 ) ;
#19073 = DIRECTION ( 'NONE',  ( 0.000000000000000000, 0.000000000000000000, 1.000000000000000000 ) ) ;
#19074 = CARTESIAN_POINT ( 'NONE',  ( 0.000000000000000000, 0.000000000000000000, 12.00000000000000000 ) ) ;
#19075 = CARTESIAN_POINT ( 'NONE',  ( -15.19790265903627180, 9.644882309621941374, 32.00000000000000000 ) ) ;
#19076 = ORIENTED_EDGE ( 'NONE', *, *, #1247, .F. ) ;
#19077 = DIRECTION ( 'NONE',  ( 1.000000000000000000, 0.000000000000000000, 0.000000000000000000 ) ) ;
#19078 =( BOUNDED_CURVE ( )  B_SPLINE_CURVE ( 2, ( #17670, #5548, #863, #18967, #16175, #9783, #11373, #19063, #14271, #12870, #14371, #14480, #6846, #9977, #2445 ),
 .UNSPECIFIED., .F., .F. ) 
 B_SPLINE_CURVE_WITH_KNOTS ( ( 3, 2, 2, 2, 2, 2, 2, 3 ),
 ( 0.000000000000000000, 0.04999999999999999584, 0.09999999999999999167, 0.1499999999999999944, 0.1999999999999999833, 0.2500000000000000000, 0.2999999999999999889, 0.3499999999999999778 ),
 .UNSPECIFIED. ) 
 CURVE ( )  GEOMETRIC_REPRESENTATION_ITEM ( )  RATIONAL_B_SPLINE_CURVE ( ( 1.000000000000000000, 0.9876883405951377704, 1.000000000000000000, 0.9876883405951377704, 1.000000000000000000, 0.9876883405951377704, 1.000000000000000000, 0.9876883405951377704, 1.000000000000000000, 0.9876883405951377704, 1.000000000000000000, 0.9876883405951377704, 1.000000000000000000, 0.9876883405951377704, 1.000000000000000000 ) ) 
 REPRESENTATION_ITEM ( '' )  );
#19079 = CARTESIAN_POINT ( 'NONE',  ( 13.00000000000000178, 3.789407127742559833, -3.087705756618140285 ) ) ;
#19080 = VECTOR ( 'NONE', #8166, 1000.000000000000000 ) ;
#19081 = VERTEX_POINT ( 'NONE', #9804 ) ;
#19082 = DIRECTION ( 'NONE',  ( 1.000000000000000000, 0.000000000000000000, 0.000000000000000000 ) ) ;
#19083 = AXIS2_PLACEMENT_3D ( 'NONE', #9516, #9416, #15514 ) ;
#19084 = DIRECTION ( 'NONE',  ( -0.000000000000000000, -1.000000000000000000, -0.000000000000000000 ) ) ;
#19085 = CARTESIAN_POINT ( 'NONE',  ( -7.937500000000000000, 4.582717761692651770, -0.7089489049740185234 ) ) ;
#19086 = CARTESIAN_POINT ( 'NONE',  ( 6.843749997951615427, -4.233219804643904460, 2.444050593749960587 ) ) ;
#19087 = LINE ( 'NONE', #17593, #17474 ) ;
#19088 = CARTESIAN_POINT ( 'NONE',  ( 13.00000000000000000, 4.333424887443004359, 2.261628166637590365 ) ) ;
#19089 = CARTESIAN_POINT ( 'NONE',  ( 2.789999999999999147, 20.70663861606272249, 15.04425356660767932 ) ) ;
#19090 = ORIENTED_EDGE ( 'NONE', *, *, #6884, .F. ) ;
#19091 = B_SPLINE_CURVE_WITH_KNOTS ( 'NONE', 3,
 ( #10863, #9070, #10765, #1560, #19665, #4462 ),
 .UNSPECIFIED., .F., .F.,
 ( 4, 2, 4 ),
 ( 2.132675795048140697E-07, 0.001878604073277005205, 0.003756994878974505639 ),
 .UNSPECIFIED. ) ;
#19092 = FACE_OUTER_BOUND ( 'NONE', #7161, .T. ) ;
#19093 = AXIS2_PLACEMENT_3D ( 'NONE', #1112, #16719, #7384 ) ;
#19094 = DIRECTION ( 'NONE',  ( 1.000000000000000000, 0.000000000000000000, 0.000000000000000000 ) ) ;
#19095 = CARTESIAN_POINT ( 'NONE',  ( 0.000000000000000000, 0.000000000000000000, 12.00000000000000000 ) ) ;
#19096 = VECTOR ( 'NONE', #11209, 1000.000000000000000 ) ;
#19097 = CARTESIAN_POINT ( 'NONE',  ( 10.96874999795161720, -3.114526743279228072, -3.846120219227966430 ) ) ;
#19098 = CARTESIAN_POINT ( 'NONE',  ( -10.00000000000000000, 0.000000000000000000, 0.000000000000000000 ) ) ;
#19099 = CARTESIAN_POINT ( 'NONE',  ( 4.080749450109649956, 4.080749450109650844, -14.81249999590322552 ) ) ;
#19100 = ORIENTED_EDGE ( 'NONE', *, *, #6817, .T. ) ;
#19101 = EDGE_CURVE ( 'NONE', #7536, #18514, #14788, .T. ) ;
#19102 = CARTESIAN_POINT ( 'NONE',  ( 9.812499995903223748, -4.080749450109678378, 4.080749450109621534 ) ) ;
#19103 = EDGE_CURVE ( 'NONE', #10889, #6099, #8998, .T. ) ;
#19104 = LINE ( 'NONE', #10109, #1495 ) ;
#19105 = B_SPLINE_CURVE_WITH_KNOTS ( 'NONE', 3,
 ( #16956, #3236, #144, #15260 ),
 .UNSPECIFIED., .F., .F.,
 ( 4, 4 ),
 ( 3.059063720760159520E-07, 0.0006888942284914164422 ),
 .UNSPECIFIED. ) ;
#19106 = EDGE_LOOP ( 'NONE', ( #5641, #18047, #5075, #1691 ) ) ;
#19107 = DIRECTION ( 'NONE',  ( 0.000000000000000000, 0.000000000000000000, 1.000000000000000000 ) ) ;
#19108 = CARTESIAN_POINT ( 'NONE',  ( -3.476417968967383754, 17.43449690031536292, -35.00000000000000000 ) ) ;
#19109 = AXIS2_PLACEMENT_3D ( 'NONE', #2188, #5477, #6873 ) ;
#19110 = CIRCLE ( 'NONE', #4417, 6.760799999999997034 ) ;
#19111 = CARTESIAN_POINT ( 'NONE',  ( 0.000000000000000000, 15.04425356660790136, -20.70663861606255196 ) ) ;
#19112 = DIRECTION ( 'NONE',  ( -1.000000000000000000, -0.000000000000000000, -0.000000000000000000 ) ) ;
#19113 = ORIENTED_EDGE ( 'NONE', *, *, #18360, .T. ) ;
#19114 = FACE_BOUND ( 'NONE', #18691, .T. ) ;
#19115 = CARTESIAN_POINT ( 'NONE',  ( -17.11901729331276911, 5.562305898749051458, 32.00000000000000000 ) ) ;
#19116 = ORIENTED_EDGE ( 'NONE', *, *, #8, .T. ) ;
#19117 = DIRECTION ( 'NONE',  ( -1.000000000000000000, -0.000000000000000000, -0.000000000000000000 ) ) ;
#19118 = ORIENTED_EDGE ( 'NONE', *, *, #7862, .T. ) ;
#19119 = B_SPLINE_CURVE_WITH_KNOTS ( 'NONE', 3,
 ( #665, #12573, #18961, #2256, #18761, #6639 ),
 .UNSPECIFIED., .F., .F.,
 ( 4, 2, 4 ),
 ( 4.462636882235905044E-07, 0.001879885203074807597, 0.003759324142461391294 ),
 .UNSPECIFIED. ) ;
#19120 = CARTESIAN_POINT ( 'NONE',  ( 13.86923836996420789, -11.47363181547641453, -35.00000000000000000 ) ) ;
#19121 = ORIENTED_EDGE ( 'NONE', *, *, #10386, .T. ) ;
#19122 = ADVANCED_FACE ( 'NONE', ( #2967 ), #19376, .T. ) ;
#19123 = CARTESIAN_POINT ( 'NONE',  ( -3.293609449816390367, 7.263869220928322434, -0.01675691374232982436 ) ) ;
#19124 = CARTESIAN_POINT ( 'NONE',  ( 0.07186815222488071586, -5.344160105508533931, -24.78765742476144140 ) ) ;
#19125 = PRODUCT_DEFINITION_SHAPE ( 'NONE', 'NONE',  #19791 ) ;
#19126 = FACE_OUTER_BOUND ( 'NONE', #6468, .T. ) ;
#19127 = AXIS2_PLACEMENT_3D ( 'NONE', #9266, #6241, #16969 ) ;
#19128 = CARTESIAN_POINT ( 'NONE',  ( 0.9027913098498565603, 5.700000000000000178, -11.50000000000000355 ) ) ;
#19129 = VERTEX_POINT ( 'NONE', #17882 ) ;
#19130 = CARTESIAN_POINT ( 'NONE',  ( 0.000000000000000000, 24.04302995059966719, 1.991882183130389228 ) ) ;
#19131 = CARTESIAN_POINT ( 'NONE',  ( 1.869200000000000195, 8.279592079675421725E-16, 6.760799999999997034 ) ) ;
#19132 = ORIENTED_EDGE ( 'NONE', *, *, #16529, .T. ) ;
#19133 = AXIS2_PLACEMENT_3D ( 'NONE', #16179, #16080, #19356 ) ;
#19134 = ADVANCED_FACE ( 'NONE', ( #19474 ), #1049, .T. ) ;
#19135 = DIRECTION ( 'NONE',  ( 0.000000000000000000, 0.000000000000000000, 1.000000000000000000 ) ) ;
#19136 = CARTESIAN_POINT ( 'NONE',  ( -6.626241948324210540, -16.73597674598852336, 32.00000000000000000 ) ) ;
#19137 = CIRCLE ( 'NONE', #10521, 1.000000000000002442 ) ;
#19138 = EDGE_LOOP ( 'NONE', ( #4294, #3068, #11408, #18152 ) ) ;
#19139 = CARTESIAN_POINT ( 'NONE',  ( -34.92499999999994742, 0.000000000000000000, 0.000000000000000000 ) ) ;
#19140 = DIRECTION ( 'NONE',  ( 1.000000000000000000, 0.000000000000000000, 0.000000000000000000 ) ) ;
#19141 = CARTESIAN_POINT ( 'NONE',  ( -2.299999999999996270, 7.470345474798878944E-16, 6.000000000000020428 ) ) ;
#19142 = EDGE_LOOP ( 'NONE', ( #12663, #1245 ) ) ;
#19143 = DIRECTION ( 'NONE',  ( 0.000000000000000000, 0.000000000000000000, 1.000000000000000000 ) ) ;
#19144 = ADVANCED_FACE ( 'NONE', ( #9081 ), #8976, .T. ) ;
#19145 = ORIENTED_EDGE ( 'NONE', *, *, #127, .F. ) ;
#19146 = CONTEXT_DEPENDENT_SHAPE_REPRESENTATION ( #6916, #6966 ) ;
#19147 = CARTESIAN_POINT ( 'NONE',  ( 0.02436607992776021470, 21.30679549418649543, -12.59161484032888723 ) ) ;
#19148 = FACE_OUTER_BOUND ( 'NONE', #2542, .T. ) ;
#19149 = DIRECTION ( 'NONE',  ( 0.000000000000000000, 0.7315216790650493905, -0.6818181818181815457 ) ) ;
#19150 = ORIENTED_EDGE ( 'NONE', *, *, #2662, .T. ) ;
#19151 = CARTESIAN_POINT ( 'NONE',  ( -2.000000000000001776, 3.218695387886217230, 3.000000000000000000 ) ) ;
#19152 = FACE_OUTER_BOUND ( 'NONE', #1808, .T. ) ;
#19153 = DIRECTION ( 'NONE',  ( 0.000000000000000000, -1.000000000000000000, 0.000000000000000000 ) ) ;
#19154 = ORIENTED_EDGE ( 'NONE', *, *, #12035, .F. ) ;
#19155 = CARTESIAN_POINT ( 'NONE',  ( 1.255998204157470211, -17.85806462366060288, 32.00000000000000000 ) ) ;
#19156 = VECTOR ( 'NONE', #19755, 1000.000000000000000 ) ;
#19157 = ORIENTED_EDGE ( 'NONE', *, *, #11944, .T. ) ;
#19158 = EDGE_CURVE ( 'NONE', #870, #2904, #10485, .T. ) ;
#19159 = FACE_OUTER_BOUND ( 'NONE', #7768, .T. ) ;
#19160 = CARTESIAN_POINT ( 'NONE',  ( -5.700000000000001066, 1.090170143537592985E-15, -9.332722423957234170 ) ) ;
#19161 = EDGE_LOOP ( 'NONE', ( #8683, #14972 ) ) ;
#19162 = DIRECTION ( 'NONE',  ( -0.000000000000000000, -0.000000000000000000, 1.000000000000000000 ) ) ;
#19163 = B_SPLINE_CURVE_WITH_KNOTS ( 'NONE', 3,
 ( #10839, #7625, #16948, #3228, #5830, #11943, #12047, #15144, #18055, #19644 ),
 .UNSPECIFIED., .F., .F.,
 ( 4, 3, 3, 4 ),
 ( 0.000000000000000000, 0.0001875345074742635904, 0.0003808595644229702693, 0.0005744879655065566939 ),
 .UNSPECIFIED. ) ;
#19164 =( NAMED_UNIT ( * ) PLANE_ANGLE_UNIT ( ) SI_UNIT ( $, .RADIAN. ) );
#19165 = EDGE_CURVE ( 'NONE', #12820, #1041, #18083, .T. ) ;
#19166 = ORIENTED_EDGE ( 'NONE', *, *, #4561, .F. ) ;
#19167 = ORIENTED_EDGE ( 'NONE', *, *, #18706, .F. ) ;
#19168 = LINE ( 'NONE', #580, #14974 ) ;
#19169 = AXIS2_PLACEMENT_3D ( 'NONE', #7411, #9139, #15040 ) ;
#19170 = AXIS2_PLACEMENT_3D ( 'NONE', #825, #13026, #1004 ) ;
#19171 = CARTESIAN_POINT ( 'NONE',  ( 1.749999999999998002, -19.67366047555515252, -20.02152543075368030 ) ) ;
#19172 = CARTESIAN_POINT ( 'NONE',  ( 0.5958122406256382009, 5.668774803599156975, -8.000000000000005329 ) ) ;
#19173 = EDGE_LOOP ( 'NONE', ( #15276, #1871, #14819, #8549, #8306, #5513, #12723, #17084 ) ) ;
#19174 = DIRECTION ( 'NONE',  ( -1.000000000000000000, 0.000000000000000000, 0.000000000000000000 ) ) ;
#19175 = CARTESIAN_POINT ( 'NONE',  ( 12.65441706489329299, 3.384649025117562271, -4.627665042997699096 ) ) ;
#19176 = VERTEX_POINT ( 'NONE', #3063 ) ;
#19177 = CARTESIAN_POINT ( 'NONE',  ( -7.626241948324210540, -16.73597674598852336, -32.00000000000000000 ) ) ;
#19178 = CARTESIAN_POINT ( 'NONE',  ( 2.718131914667133220, -10.24630254990500511, -23.19485392143224445 ) ) ;
#19179 = CARTESIAN_POINT ( 'NONE',  ( 3.968750000000007994, 6.874076642538976323, 0.000000000000000000 ) ) ;
#19180 = CARTESIAN_POINT ( 'NONE',  ( 11.84374999795161365, -2.444050593749961031, -4.233219804643904460 ) ) ;
#19181 = CARTESIAN_POINT ( 'NONE',  ( 7.312499995903225525, 4.936344801571289409, 2.850000000000024070 ) ) ;
#19182 = SURFACE_SIDE_STYLE ('',( #889 ) ) ;
#19183 = CARTESIAN_POINT ( 'NONE',  ( -2.000000000000000000, 4.999999999999998224, 37.99999999999999289 ) ) ;
#19184 = ADVANCED_FACE ( 'NONE', ( #16488, #13373 ), #4177, .F. ) ;
#19185 = ORIENTED_EDGE ( 'NONE', *, *, #5000, .F. ) ;
#19186 = DIRECTION ( 'NONE',  ( -1.000000000000000000, -0.000000000000000000, -0.000000000000000000 ) ) ;
#19187 = DIRECTION ( 'NONE',  ( 0.000000000000000000, 0.000000000000000000, -1.000000000000000000 ) ) ;
#19188 = UNCERTAINTY_MEASURE_WITH_UNIT (LENGTH_MEASURE( 1.000000000000000082E-05 ), #14367, 'distance_accuracy_value', 'NONE');
#19189 = FACE_OUTER_BOUND ( 'NONE', #16251, .T. ) ;
#19190 =( BOUNDED_SURFACE ( )  B_SPLINE_SURFACE ( 1, 2, ( 
 ( #6023, #18147, #10543, #4340, #10255, #13339, #19736, #3026, #13640, #2923, #1236, #8845, #11942, #5726, #14944, #9040, #1333 ),
 ( #5926, #15143, #7216, #2728, #1438, #1145, #12046, #11746, #7316, #13435, #10355, #7415, #13540, #16452, #19341, #14752, #7520 ) ),
 .UNSPECIFIED., .F., .F., .F. ) 
 B_SPLINE_SURFACE_WITH_KNOTS ( ( 2, 2 ),
 ( 3, 2, 2, 2, 2, 2, 2, 2, 3 ),
 ( 0.000000000000000000, 1.000000000000000000 ),
 ( 0.000000000000000000, 0.05000000000000000278, 0.1000000000000000056, 0.1499999999999999944, 0.2000000000000000111, 0.2500000000000000000, 0.2999999999999999889, 0.3499999999999999778, 0.4000000000000000222 ),
 .UNSPECIFIED. ) 
 GEOMETRIC_REPRESENTATION_ITEM ( )  RATIONAL_B_SPLINE_SURFACE ( (
 ( 1.000000000000000000, 0.9876883405951377704, 1.000000000000000000, 0.9876883405951377704, 1.000000000000000000, 0.9876883405951377704, 1.000000000000000000, 0.9876883405951377704, 1.000000000000000000, 0.9876883405951377704, 1.000000000000000000, 0.9876883405951377704, 1.000000000000000000, 0.9876883405951377704, 1.000000000000000000, 0.9876883405951377704, 1.000000000000000000),
 ( 1.000000000000000000, 0.9876883405951377704, 1.000000000000000000, 0.9876883405951377704, 1.000000000000000000, 0.9876883405951377704, 1.000000000000000000, 0.9876883405951377704, 1.000000000000000000, 0.9876883405951377704, 1.000000000000000000, 0.9876883405951377704, 1.000000000000000000, 0.9876883405951377704, 1.000000000000000000, 0.9876883405951377704, 1.000000000000000000) ) ) 
 REPRESENTATION_ITEM ( '' )  SURFACE ( )  );
#19191 = DIRECTION ( 'NONE',  ( 0.000000000000000000, 0.000000000000000000, 1.000000000000000000 ) ) ;
#19192 = AXIS2_PLACEMENT_3D ( 'NONE', #17515, #5203, #3901 ) ;
#19193 =( REPRESENTATION_RELATIONSHIP ('NONE','NONE', #18211, #10045 ) REPRESENTATION_RELATIONSHIP_WITH_TRANSFORMATION ( #18851 )SHAPE_REPRESENTATION_RELATIONSHIP( ) );
#19194 = CARTESIAN_POINT ( 'NONE',  ( -1.988169868018624609, -4.465502636338009701, -9.843749997951615427 ) ) ;
#19195 = EDGE_LOOP ( 'NONE', ( #13530, #1017 ) ) ;
#19196 = CARTESIAN_POINT ( 'NONE',  ( 11.84374999795161365, -4.888101187500000222, -3.383411828340740850E-14 ) ) ;
#19197 = CARTESIAN_POINT ( 'NONE',  ( 2.850000000000024070, 4.936344801571289409, -7.312499995903225525 ) ) ;
#19198 = EDGE_LOOP ( 'NONE', ( #15382, #17736, #13275, #8868 ) ) ;
#19199 = ADVANCED_FACE ( 'NONE', ( #1568 ), #18943, .T. ) ;
#19200 = LINE ( 'NONE', #8514, #16 ) ;
#19201 = CARTESIAN_POINT ( 'NONE',  ( 0.8944271909999176318, 8.327598234201999146E-16, -6.799999999999998046 ) ) ;
#19202 = DIRECTION ( 'NONE',  ( -0.000000000000000000, -0.000000000000000000, -1.000000000000000000 ) ) ;
#19203 = EDGE_CURVE ( 'NONE', #4244, #1462, #7055, .T. ) ;
#19204 = VERTEX_POINT ( 'NONE', #11878 ) ;
#19205 = VECTOR ( 'NONE', #743, 1000.000000000000000 ) ;
#19206 = AXIS2_PLACEMENT_3D ( 'NONE', #5028, #8130, #17238 ) ;
#19207 = DIRECTION ( 'NONE',  ( 1.000000000000000000, 0.000000000000000000, 0.000000000000000000 ) ) ;
#19208 = FACE_OUTER_BOUND ( 'NONE', #10346, .T. ) ;
#19209 = VECTOR ( 'NONE', #7022, 1000.000000000000000 ) ;
#19210 = CARTESIAN_POINT ( 'NONE',  ( 7.468749997951615427, -1.510506337161893864, 4.648860486681943627 ) ) ;
#19211 = ORIENTED_EDGE ( 'NONE', *, *, #4960, .T. ) ;
#19212 = EDGE_CURVE ( 'NONE', #8201, #9486, #16170, .T. ) ;
#19213 = CARTESIAN_POINT ( 'NONE',  ( 10.81249999590322375, -4.840010801796461593, -3.143139765844656264 ) ) ;
#19214 = VERTEX_POINT ( 'NONE', #1472 ) ;
#19215 = CARTESIAN_POINT ( 'NONE',  ( 17.68117051311639898, -3.372863662543048591, 32.00000000000000000 ) ) ;
#19216 = CARTESIAN_POINT ( 'NONE',  ( 2.031033491000349134, 24.80232951178394885, -12.05173163741697451 ) ) ;
#19217 = DIRECTION ( 'NONE',  ( 0.000000000000000000, 0.000000000000000000, -1.000000000000000000 ) ) ;
#19218 = FACE_BOUND ( 'NONE', #5562, .T. ) ;
#19219 = ORIENTED_EDGE ( 'NONE', *, *, #18271, .F. ) ;
#19220 = FACE_BOUND ( 'NONE', #4444, .T. ) ;
#19221 = EDGE_CURVE ( 'NONE', #19054, #15416, #2319, .T. ) ;
#19222 = DIRECTION ( 'NONE',  ( 0.000000000000000000, 0.000000000000000000, 1.000000000000000000 ) ) ;
#19223 = CIRCLE ( 'NONE', #16357, 1.000000000000002665 ) ;
#19224 = ORIENTED_EDGE ( 'NONE', *, *, #18328, .T. ) ;
#19225 = VECTOR ( 'NONE', #1395, 1000.000000000000000 ) ;
#19226 = VECTOR ( 'NONE', #4501, 1000.000000000000000 ) ;
#19227 = ADVANCED_FACE ( 'NONE', ( #19674 ), #4275, .F. ) ;
#19228 = AXIS2_PLACEMENT_3D ( 'NONE', #1084, #7160, #14508 ) ;
#19229 = DIRECTION ( 'NONE',  ( 0.000000000000000000, 0.000000000000000000, 1.000000000000000000 ) ) ;
#19230 = CARTESIAN_POINT ( 'NONE',  ( 4.648860486681943627, -1.510506337161893864, -7.843749997951614539 ) ) ;
#19231 = ORIENTED_EDGE ( 'NONE', *, *, #4434, .F. ) ;
#19232 = CARTESIAN_POINT ( 'NONE',  ( -7.937500000000000000, -4.582717761692664205, -0.7089489049740167470 ) ) ;
#19233 = CARTESIAN_POINT ( 'NONE',  ( -2.620002426024580000, -5.142044285764733935, -12.50000000000000533 ) ) ;
#19234 = ORIENTED_EDGE ( 'NONE', *, *, #10234, .F. ) ;
#19235 = DIRECTION ( 'NONE',  ( 0.000000000000000000, 0.000000000000000000, 1.000000000000000000 ) ) ;
#19236 = CIRCLE ( 'NONE', #3585, 1.000000000000000888 ) ;
#19237 = ORIENTED_EDGE ( 'NONE', *, *, #15745, .T. ) ;
#19238 = AXIS2_PLACEMENT_3D ( 'NONE', #10382, #2757, #14877 ) ;
#19239 = CARTESIAN_POINT ( 'NONE',  ( 0.000000000000000000, 0.000000000000000000, -6.527800000000000047 ) ) ;
#19240 = CARTESIAN_POINT ( 'NONE',  ( 2.765633920072236851, -22.71065055754445439, -9.836394144775947979 ) ) ;
#19241 = AXIS2_PLACEMENT_3D ( 'NONE', #7363, #10401, #19191 ) ;
#19242 = DIRECTION ( 'NONE',  ( 0.000000000000000000, 0.000000000000000000, -1.000000000000000000 ) ) ;
#19243 = EDGE_LOOP ( 'NONE', ( #17512, #14755, #18743, #18825, #9258, #12374, #3854, #10620 ) ) ;
#19244 = CARTESIAN_POINT ( 'NONE',  ( 4.648860486681943627, -1.510506337161893864, -7.468749997951615427 ) ) ;
#19245 = CARTESIAN_POINT ( 'NONE',  ( 9.812499995903225525, -4.080749450109678378, 4.080749450109622423 ) ) ;
#19246 = CARTESIAN_POINT ( 'NONE',  ( -11.00000000000000355, -3.278623949159159778, 2.625000000000000888 ) ) ;
#19247 = ORIENTED_EDGE ( 'NONE', *, *, #13470, .F. ) ;
#19248 = ADVANCED_FACE ( 'NONE', ( #11978 ), #7352, .T. ) ;
#19249 = CIRCLE ( 'NONE', #2633, 1.000000000000002665 ) ;
#19250 = DIRECTION ( 'NONE',  ( -0.000000000000000000, -0.000000000000000000, 1.000000000000000000 ) ) ;
#19251 = AXIS2_PLACEMENT_3D ( 'NONE', #14503, #8285, #17397 ) ;
#19252 = VERTEX_POINT ( 'NONE', #4469 ) ;
#19253 = CIRCLE ( 'NONE', #2010, 3.000000000000000000 ) ;
#19254 = AXIS2_PLACEMENT_3D ( 'NONE', #12745, #8336, #5329 ) ;
#19255 = CARTESIAN_POINT ( 'NONE',  ( 6.234374998975811266, 4.584782303107579615, 2.647025296875021638 ) ) ;
#19256 = DIRECTION ( 'NONE',  ( -0.000000000000000000, -0.000000000000000000, -1.000000000000000000 ) ) ;
#19257 = EDGE_LOOP ( 'NONE', ( #7285, #4768 ) ) ;
#19258 = CARTESIAN_POINT ( 'NONE',  ( -2.444050593750049849, -4.233219804643852946, -6.843749997951615427 ) ) ;
#19259 = PRESENTATION_STYLE_ASSIGNMENT (( #6946 ) ) ;
#19260 = CYLINDRICAL_SURFACE ( 'NONE', #12869, 13.20000000000000284 ) ;
#19261 = EDGE_LOOP ( 'NONE', ( #18541, #5623, #19224, #13320 ) ) ;
#19262 = ORIENTED_EDGE ( 'NONE', *, *, #4815, .T. ) ;
#19263 = DIRECTION ( 'NONE',  ( 1.000000000000000000, 0.000000000000000000, 0.000000000000000000 ) ) ;
#19264 = CIRCLE ( 'NONE', #6463, 6.500000000000002665 ) ;
#19265 = CARTESIAN_POINT ( 'NONE',  ( 0.006931111373678920488, 22.53293026234503316, 9.685942809247130469 ) ) ;
#19266 = EDGE_CURVE ( 'NONE', #5485, #4917, #12555, .T. ) ;
#19267 = ORIENTED_EDGE ( 'NONE', *, *, #15331, .F. ) ;
#19268 = CARTESIAN_POINT ( 'NONE',  ( 0.1882239034349757756, -12.84621645676860702, 22.54313264455009147 ) ) ;
#19269 = ORIENTED_EDGE ( 'NONE', *, *, #13372, .T. ) ;
#19270 = DIRECTION ( 'NONE',  ( 1.000000000000000000, 6.419766481290786633E-33, -0.000000000000000000 ) ) ;
#19271 = AXIS2_PLACEMENT_3D ( 'NONE', #14220, #314, #14117 ) ;
#19272 = CARTESIAN_POINT ( 'NONE',  ( 8.843749997951615427, -1.988169868018530462, -4.465502636338051445 ) ) ;
#19273 = EDGE_LOOP ( 'NONE', ( #8771, #2610 ) ) ;
#19274 = DIRECTION ( 'NONE',  ( 1.000000000000000000, 0.000000000000000000, 0.000000000000000000 ) ) ;
#19275 = ADVANCED_FACE ( 'NONE', ( #12176 ), #18281, .T. ) ;
#19276 = APPLICATION_CONTEXT ( 'automotive_design' ) ;
#19277 = DIRECTION ( 'NONE',  ( -9.559896011775280412E-17, 0.7806247497997995666, -0.6250000000000002220 ) ) ;
#19278 = CARTESIAN_POINT ( 'NONE',  ( 1.394999999999999574, -25.12109765559663188, 12.52377138324214378 ) ) ;
#19279 = CARTESIAN_POINT ( 'NONE',  ( 7.843749997951614539, -4.781284448697200595, 1.016293382781377819 ) ) ;
#19280 = PRODUCT_DEFINITION_SHAPE ( 'NONE', 'NONE',  #19783 ) ;
#19281 = ADVANCED_FACE ( 'NONE', ( #3263 ), #734, .T. ) ;
#19282 = DIRECTION ( 'NONE',  ( 0.000000000000000000, 0.000000000000000000, -1.000000000000000000 ) ) ;
#19283 = AXIS2_PLACEMENT_3D ( 'NONE', #384, #2081, #8082 ) ;
#19284 = ORIENTED_EDGE ( 'NONE', *, *, #4165, .T. ) ;
#19285 = CARTESIAN_POINT ( 'NONE',  ( 0.000000000000000000, 0.000000000000000000, -29.00000000000000000 ) ) ;
#19286 = DIRECTION ( 'NONE',  ( -1.000000000000000000, -0.000000000000000000, -0.000000000000000000 ) ) ;
#19287 = CARTESIAN_POINT ( 'NONE',  ( 6.656249997951614539, -4.936344801571327601, 2.849999999999954348 ) ) ;
#19288 = FACE_OUTER_BOUND ( 'NONE', #2126, .T. ) ;
#19289 = AXIS2_PLACEMENT_3D ( 'NONE', #2665, #8783, #3984 ) ;
#19290 = CARTESIAN_POINT ( 'NONE',  ( 2.601776144743012775, -10.68696068830424473, 23.64332819722378076 ) ) ;
#19291 = ORIENTED_EDGE ( 'NONE', *, *, #19071, .T. ) ;
#19292 = DIRECTION ( 'NONE',  ( 0.000000000000000000, 0.000000000000000000, 1.000000000000000000 ) ) ;
#19293 = DIRECTION ( 'NONE',  ( -1.000000000000000000, -0.000000000000000000, -0.000000000000000000 ) ) ;
#19294 = ORIENTED_EDGE ( 'NONE', *, *, #12082, .F. ) ;
#19295 = CARTESIAN_POINT ( 'NONE',  ( 15.31249999590322552, -5.668774803599162304, 0.5958122406255995651 ) ) ;
#19296 = EDGE_CURVE ( 'NONE', #3019, #16293, #6347, .T. ) ;
#19297 = CIRCLE ( 'NONE', #10055, 3.000000000000000000 ) ;
#19298 = CARTESIAN_POINT ( 'NONE',  ( 1.039999999999996927, 4.633866840649313090, -27.68468304288253634 ) ) ;
#19299 = CARTESIAN_POINT ( 'NONE',  ( 0.000000000000000000, 0.000000000000000000, 0.000000000000000000 ) ) ;
#19300 = CARTESIAN_POINT ( 'NONE',  ( 1.749999999999998002, 0.000000000000000000, 0.000000000000000000 ) ) ;
#19301 = ORIENTED_EDGE ( 'NONE', *, *, #15691, .F. ) ;
#19302 = AXIS2_PLACEMENT_3D ( 'NONE', #13070, #14765, #2260 ) ;
#19303 = CARTESIAN_POINT ( 'NONE',  ( 5.000000000000000000, 1.999999999999998224, 41.99999999999999289 ) ) ;
#19304 = CARTESIAN_POINT ( 'NONE',  ( 2.765633920072235519, -18.55949924794880346, -16.37294372382878649 ) ) ;
#19305 = DIRECTION ( 'NONE',  ( 0.000000000000000000, 0.000000000000000000, 1.000000000000000000 ) ) ;
#19306 = ORIENTED_EDGE ( 'NONE', *, *, #17415, .F. ) ;
#19307 =( BOUNDED_CURVE ( )  B_SPLINE_CURVE ( 2, ( #13613, #19614, #15117, #10516, #16614, #5995, #1114, #4211, #7188, #5901, #7493, #3001, #6093, #15218, #8814 ),
 .UNSPECIFIED., .F., .F. ) 
 B_SPLINE_CURVE_WITH_KNOTS ( ( 3, 2, 2, 2, 2, 2, 2, 3 ),
 ( 0.000000000000000000, 0.05000000000000000278, 0.1000000000000000056, 0.1499999999999999944, 0.2000000000000000111, 0.2500000000000000000, 0.2999999999999999889, 0.3265529187307101844 ),
 .UNSPECIFIED. ) 
 CURVE ( )  GEOMETRIC_REPRESENTATION_ITEM ( )  RATIONAL_B_SPLINE_CURVE ( ( 1.000000000000000000, 0.9876883405951377704, 1.000000000000000000, 0.9876883405951377704, 1.000000000000000000, 0.9876883405951377704, 1.000000000000000000, 0.9876883405951377704, 1.000000000000000000, 0.9876883405951377704, 1.000000000000000000, 0.9876883405951377704, 1.000000000000000000, 0.9934617901676502383, 0.9938679225082089896 ) ) 
 REPRESENTATION_ITEM ( '' )  );
#19308 = CARTESIAN_POINT ( 'NONE',  ( 6.656249997951614539, 0.000000000000000000, -4.888101187500000222 ) ) ;
#19309 = ORIENTED_EDGE ( 'NONE', *, *, #4528, .F. ) ;
#19310 = CARTESIAN_POINT ( 'NONE',  ( -41.99999999999999289, -5.000000000000001776, -5.000000000000000000 ) ) ;
#19311 = CIRCLE ( 'NONE', #2376, 1.000000000000003553 ) ;
#19312 = CARTESIAN_POINT ( 'NONE',  ( 0.7589665349472707323, -4.828387785247840291, -27.14933624560912762 ) ) ;
#19313 = EDGE_CURVE ( 'NONE', #12253, #17067, #6772, .T. ) ;
#19314 = DIRECTION ( 'NONE',  ( 0.000000000000000000, 0.000000000000000000, -1.000000000000000000 ) ) ;
#19315 = DIRECTION ( 'NONE',  ( 0.000000000000000000, 1.776356839400250465E-15, 1.000000000000000000 ) ) ;
#19316 = VERTEX_POINT ( 'NONE', #17177 ) ;
#19317 = CARTESIAN_POINT ( 'NONE',  ( -4.781284448697201483, -1.016293382781378485, -12.84374999795161543 ) ) ;
#19318 = CARTESIAN_POINT ( 'NONE',  ( 6.000000000000005329, 5.388445916248354013E-16, -4.400000000000000355 ) ) ;
#19319 = EDGE_CURVE ( 'NONE', #18587, #6920, #8026, .T. ) ;
#19320 = VECTOR ( 'NONE', #7129, 1000.000000000000000 ) ;
#19321 = EDGE_LOOP ( 'NONE', ( #15244, #8847, #9864, #11772 ) ) ;
#19322 = ADVANCED_FACE ( 'NONE', ( #4764 ), #15774, .F. ) ;
#19323 = B_SPLINE_CURVE_WITH_KNOTS ( 'NONE', 1,
 ( #9650, #6615 ),
 .UNSPECIFIED., .F., .F.,
 ( 2, 2 ),
 ( 0.000000000000000000, 1.000000000000000000 ),
 .UNSPECIFIED. ) ;
#19324 = CARTESIAN_POINT ( 'NONE',  ( 0.000000000000000000, 5.535312321042724193, 23.48180575137730841 ) ) ;
#19325 = CARTESIAN_POINT ( 'NONE',  ( 5.700000000000001066, -3.980288726281172656E-14, -7.312499995903225525 ) ) ;
#19326 = VERTEX_POINT ( 'NONE', #6159 ) ;
#19327 = CARTESIAN_POINT ( 'NONE',  ( 13.00000000000000533, 4.859449410165161964, -2.460251518383709257 ) ) ;
#19328 = CARTESIAN_POINT ( 'NONE',  ( -3.350375938067128967, -4.611396867937178179, -13.00000000000000533 ) ) ;
#19329 = CARTESIAN_POINT ( 'NONE',  ( 0.02436607992776498519, -21.30679549418621832, -12.59161484032935618 ) ) ;
#19330 = ORIENTED_EDGE ( 'NONE', *, *, #1955, .F. ) ;
#19331 = LINE ( 'NONE', #15855, #17906 ) ;
#19332 = ORIENTED_EDGE ( 'NONE', *, *, #1949, .T. ) ;
#19333 = CARTESIAN_POINT ( 'NONE',  ( 1.799999999999999600, 0.000000000000000000, 0.000000000000000000 ) ) ;
#19334 = CIRCLE ( 'NONE', #18692, 3.968750000000000000 ) ;
#19335 = EDGE_LOOP ( 'NONE', ( #1882, #9233, #18877, #18908, #7447, #11569, #96, #7041 ) ) ;
#19336 = CARTESIAN_POINT ( 'NONE',  ( 1.039999999999997593, 0.000000000000000000, 0.000000000000000000 ) ) ;
#19337 = CARTESIAN_POINT ( 'NONE',  ( 0.5745956068257360716, -5.466912017135475033, -14.11718749948790830 ) ) ;
#19338 = CARTESIAN_POINT ( 'NONE',  ( -15.00000000000000355, -8.000000000000000000, 9.797174393178825657E-16 ) ) ;
#19339 = ORIENTED_EDGE ( 'NONE', *, *, #18739, .T. ) ;
#19340 = CARTESIAN_POINT ( 'NONE',  ( 0.000000000000000000, 0.000000000000000000, -0.5557897334539606549 ) ) ;
#19341 = CARTESIAN_POINT ( 'NONE',  ( 13.00000000000000533, 0.5958122406256767256, -5.668774803599153422 ) ) ;
#19342 = PLANE ( 'NONE',  #2778 ) ;
#19343 = ORIENTED_EDGE ( 'NONE', *, *, #11980, .F. ) ;
#19344 = PLANE ( 'NONE',  #16453 ) ;
#19345 = ADVANCED_FACE ( 'NONE', ( #17077 ), #3367, .F. ) ;
#19346 = EDGE_CURVE ( 'NONE', #2096, #7371, #1695, .T. ) ;
#19347 = CIRCLE ( 'NONE', #14248, 1.000000000000000000 ) ;
#19348 = ORIENTED_EDGE ( 'NONE', *, *, #3360, .F. ) ;
#19349 = AXIS2_PLACEMENT_3D ( 'NONE', #5855, #19464, #11972 ) ;
#19350 = DIRECTION ( 'NONE',  ( 0.000000000000000000, 0.000000000000000000, 1.000000000000000000 ) ) ;
#19351 = LINE ( 'NONE', #3958, #6349 ) ;
#19352 = ADVANCED_FACE ( 'NONE', ( #9575 ), #10331, .T. ) ;
#19353 = DIRECTION ( 'NONE',  ( 0.000000000000000000, 0.000000000000000000, 1.000000000000000000 ) ) ;
#19354 = EDGE_LOOP ( 'NONE', ( #12031, #16143, #2703, #752 ) ) ;
#19355 = CARTESIAN_POINT ( 'NONE',  ( -1.988169868018530906, 4.465502636338051445, -13.46874999795161543 ) ) ;
#19356 = DIRECTION ( 'NONE',  ( 1.000000000000000000, 0.000000000000000000, 0.000000000000000000 ) ) ;
#19357 = CARTESIAN_POINT ( 'NONE',  ( 3.814044456245502701, 4.235925505221138643, -10.00000000000000533 ) ) ;
#19358 = VERTEX_POINT ( 'NONE', #9378 ) ;
#19359 = EDGE_LOOP ( 'NONE', ( #7549, #11233, #12261, #14053 ) ) ;
#19360 = CARTESIAN_POINT ( 'NONE',  ( 0.02436607992776368414, -9.836394144775550075, -22.71065055754462492 ) ) ;
#19361 = ADVANCED_FACE ( 'NONE', ( #168 ), #18376, .F. ) ;
#19362 = AXIS2_PLACEMENT_3D ( 'NONE', #17738, #19140, #14450 ) ;
#19363 = CARTESIAN_POINT ( 'NONE',  ( 0.02436607992775761261, 22.71065055754452544, 9.836394144775786330 ) ) ;
#19364 = EDGE_CURVE ( 'NONE', #14825, #5362, #9691, .T. ) ;
#19365 = CIRCLE ( 'NONE', #193, 5.400000000000000355 ) ;
#19366 = VERTEX_POINT ( 'NONE', #472 ) ;
#19367 = CARTESIAN_POINT ( 'NONE',  ( 4.936344801571308061, 2.849999999999989431, -11.00000000000000711 ) ) ;
#19368 = ORIENTED_EDGE ( 'NONE', *, *, #11980, .T. ) ;
#19369 = CARTESIAN_POINT ( 'NONE',  ( 2.000000000000001776, 0.000000000000000000, -8.265000000000021885 ) ) ;
#19370 = CARTESIAN_POINT ( 'NONE',  ( 9.312499995903225525, -2.318398865532001363, -5.207209108562852684 ) ) ;
#19371 = AXIS2_PLACEMENT_3D ( 'NONE', #12185, #18291, #13784 ) ;
#19372 = ORIENTED_EDGE ( 'NONE', *, *, #8647, .T. ) ;
#19373 = CARTESIAN_POINT ( 'NONE',  ( 2.765633920072236851, 24.15498966839963302, 5.391175441198700291 ) ) ;
#19374 = VECTOR ( 'NONE', #7280, 1000.000000000000000 ) ;
#19375 = VECTOR ( 'NONE', #7369, 1000.000000000000000 ) ;
#19376 = CYLINDRICAL_SURFACE ( 'NONE', #1680, 28.06981291497571362 ) ;
#19377 = EDGE_CURVE ( 'NONE', #725, #16376, #11281, .T. ) ;
#19378 = CARTESIAN_POINT ( 'NONE',  ( 14.84374999795161543, 2.873153789725825913, 3.954556930911861112 ) ) ;
#19379 = CARTESIAN_POINT ( 'NONE',  ( 2.765633920072233742, -24.15498966839966855, 5.391175441198523544 ) ) ;
#19380 = CARTESIAN_POINT ( 'NONE',  ( -1.799999999999999600, 0.000000000000000000, -4.000000000000000000 ) ) ;
#19381 = DIRECTION ( 'NONE',  ( -1.000000000000000000, -0.000000000000000000, -0.000000000000000000 ) ) ;
#19382 = ORIENTED_EDGE ( 'NONE', *, *, #18937, .T. ) ;
#19383 = DIRECTION ( 'NONE',  ( 0.000000000000000000, 0.000000000000000000, 1.000000000000000000 ) ) ;
#19384 = EDGE_CURVE ( 'NONE', #4160, #8623, #12674, .T. ) ;
#19385 = CARTESIAN_POINT ( 'NONE',  ( 50.00050000000000239, 0.000000000000000000, 4.000000000000000000 ) ) ;
#19386 = CARTESIAN_POINT ( 'NONE',  ( -0.5958122406255597081, 5.668774803599165857, -14.00000000000000533 ) ) ;
#19387 = ADVANCED_FACE ( 'NONE', ( #5060 ), #3558, .F. ) ;
#19388 = LINE ( 'NONE', #4386, #15094 ) ;
#19389 = AXIS2_PLACEMENT_3D ( 'NONE', #5063, #475, #12873 ) ;
#19390 = CARTESIAN_POINT ( 'NONE',  ( -3.490243377569957047E-16, 5.700000000000001066, -12.31249999590322552 ) ) ;
#19391 = AXIS2_PLACEMENT_3D ( 'NONE', #1923, #3524, #12733 ) ;
#19392 = ORIENTED_EDGE ( 'NONE', *, *, #12270, .T. ) ;
#19393 = DIRECTION ( 'NONE',  ( 0.000000000000000000, 0.000000000000000000, -1.000000000000000000 ) ) ;
#19394 = CARTESIAN_POINT ( 'NONE',  ( 2.000000000000001776, 8.247996192257451316E-16, 6.735000000000022524 ) ) ;
#19395 = APPLICATION_CONTEXT ( 'automotive_design' ) ;
#19396 = ORIENTED_EDGE ( 'NONE', *, *, #11581, .F. ) ;
#19397 = CARTESIAN_POINT ( 'NONE',  ( 10.84374999795161543, -1.016293382781444654, 4.781284448697187273 ) ) ;
#19398 = EDGE_CURVE ( 'NONE', #17936, #14330, #11172, .T. ) ;
#19399 = CARTESIAN_POINT ( 'NONE',  ( 12.00000000000000000, 4.401380596135586802E-16, -3.593999999999999861 ) ) ;
#19400 = CARTESIAN_POINT ( 'NONE',  ( -17.96448111170888851, 1.130229351527647585, -35.00000000000000000 ) ) ;
#19401 = LINE ( 'NONE', #8419, #11624 ) ;
#19402 = EDGE_LOOP ( 'NONE', ( #9407, #5943, #15840, #7679 ) ) ;
#19403 = VECTOR ( 'NONE', #15536, 1000.000000000000000 ) ;
#19404 = CARTESIAN_POINT ( 'NONE',  ( 8.468749997951615427, 2.873153789725825469, -3.954556930911862000 ) ) ;
#19405 =( NAMED_UNIT ( * ) SI_UNIT ( $, .STERADIAN. ) SOLID_ANGLE_UNIT ( ) );
#19406 = CARTESIAN_POINT ( 'NONE',  ( 4.780397808154265960, 1.280903732194420996, -9.343749997951615427 ) ) ;
#19407 = AXIS2_PLACEMENT_3D ( 'NONE', #16371, #10474, #10377 ) ;
#19408 = CARTESIAN_POINT ( 'NONE',  ( 13.00000000000000178, 0.000000000000000000, 0.000000000000000000 ) ) ;
#19409 = ORIENTED_EDGE ( 'NONE', *, *, #2426, .T. ) ;
#19410 = CARTESIAN_POINT ( 'NONE',  ( -4.500000000000000000, 0.000000000000000000, -33.00000000000000000 ) ) ;
#19411 = ORIENTED_EDGE ( 'NONE', *, *, #12460, .F. ) ;
#19412 = CARTESIAN_POINT ( 'NONE',  ( 10.58013454126452046, -14.56230589874905412, -32.00000000000000000 ) ) ;
#19413 = EDGE_CURVE ( 'NONE', #11964, #14953, #2636, .T. ) ;
#19414 = CARTESIAN_POINT ( 'NONE',  ( 7.343749997951615427, 0.7741991708318887166, -4.888101187500000222 ) ) ;
#19415 = DIRECTION ( 'NONE',  ( -1.000000000000000000, -0.000000000000000000, -0.000000000000000000 ) ) ;
#19416 = DIRECTION ( 'NONE',  ( -1.000000000000000000, -0.000000000000000000, -0.000000000000000000 ) ) ;
#19417 = EDGE_LOOP ( 'NONE', ( #10954, #8980, #625, #11575 ) ) ;
#19418 = B_SPLINE_CURVE_WITH_KNOTS ( 'NONE', 3,
 ( #7109, #19327, #16630, #4227 ),
 .UNSPECIFIED., .F., .F.,
 ( 4, 4 ),
 ( 0.000000000000000000, 0.001125480700308659687 ),
 .UNSPECIFIED. ) ;
#19419 = CARTESIAN_POINT ( 'NONE',  ( -13.86923836996420967, -11.47363181547641275, -32.00000000000000000 ) ) ;
#19420 = DIRECTION ( 'NONE',  ( -1.000000000000000000, 0.000000000000000000, 0.000000000000000000 ) ) ;
#19421 = VERTEX_POINT ( 'NONE', #1668 ) ;
#19422 = CIRCLE ( 'NONE', #18469, 1.000000000000000888 ) ;
#19423 = DIRECTION ( 'NONE',  ( 0.000000000000000000, 0.000000000000000000, 1.000000000000000000 ) ) ;
#19424 = EDGE_CURVE ( 'NONE', #10056, #19582, #9273, .T. ) ;
#19425 = CARTESIAN_POINT ( 'NONE',  ( -3.945386292505473391E-14, -5.700000000000001066, -12.31249999590322552 ) ) ;
#19426 =( BOUNDED_CURVE ( )  B_SPLINE_CURVE ( 2, ( #12030, #12331, #6008, #4512, #10629, #3116, #3014, #16934, #18134, #8828, #13418, #9025, #14931, #4322, #8925, #1320, #13724 ),
 .UNSPECIFIED., .F., .F. ) 
 B_SPLINE_CURVE_WITH_KNOTS ( ( 3, 2, 2, 2, 2, 2, 2, 2, 3 ),
 ( 0.000000000000000000, 0.05000000000000000971, 0.1000000000000000194, 0.1499999999999999944, 0.2000000000000000389, 0.2500000000000000000, 0.2999999999999999889, 0.3499999999999999223, 0.4000000000000000777 ),
 .UNSPECIFIED. ) 
 CURVE ( )  GEOMETRIC_REPRESENTATION_ITEM ( )  RATIONAL_B_SPLINE_CURVE ( ( 1.000000000000000000, 0.9876883405951377704, 1.000000000000000000, 0.9876883405951377704, 1.000000000000000000, 0.9876883405951377704, 1.000000000000000000, 0.9876883405951377704, 1.000000000000000000, 0.9876883405951377704, 1.000000000000000000, 0.9876883405951377704, 1.000000000000000000, 0.9876883405951377704, 1.000000000000000000, 0.9876883405951377704, 1.000000000000000000 ) ) 
 REPRESENTATION_ITEM ( '' )  );
#19427 = EDGE_LOOP ( 'NONE', ( #19570, #8459 ) ) ;
#19428 = CARTESIAN_POINT ( 'NONE',  ( 4.942249507334556924, 0.2590123213420971182, -12.96874999795161543 ) ) ;
#19429 = CARTESIAN_POINT ( 'NONE',  ( 13.34374999795161365, 0.2590123213420975623, 4.942249507334556924 ) ) ;
#19430 = VERTEX_POINT ( 'NONE', #9884 ) ;
#19431 = CARTESIAN_POINT ( 'NONE',  ( 2.789999999999999147, -24.44424927289185590, 0.2301004812056573479 ) ) ;
#19432 = ORIENTED_EDGE ( 'NONE', *, *, #11628, .F. ) ;
#19434 = DIRECTION ( 'NONE',  ( 0.000000000000000000, -1.000000000000000000, 0.000000000000000000 ) ) ;
#19433 = CIRCLE ( 'NONE', #12737, 6.000000000000000888 ) ;
#19435 = ORIENTED_EDGE ( 'NONE', *, *, #18352, .F. ) ;
#19436 = DIRECTION ( 'NONE',  ( 0.000000000000000000, 0.000000000000000000, 1.000000000000000000 ) ) ;
#19437 = EDGE_CURVE ( 'NONE', #5161, #8660, #15104, .T. ) ;
#19438 = FACE_OUTER_BOUND ( 'NONE', #19243, .T. ) ;
#19439 = CARTESIAN_POINT ( 'NONE',  ( 2.789999999999999147, 2.336989772644269436, 24.63872515616083447 ) ) ;
#19440 = DIRECTION ( 'NONE',  ( -0.8660254037844380415, 0.5000000000000009992, 0.000000000000000000 ) ) ;
#19441 = FACE_OUTER_BOUND ( 'NONE', #6206, .T. ) ;
#19442 = VERTEX_POINT ( 'NONE', #10167 ) ;
#19443 = LINE ( 'NONE', #11557, #15176 ) ;
#19444 = PRODUCT ( 'DUST CUP', 'DUST CUP', '', ( #15463 ) ) ;
#19445 = CIRCLE ( 'NONE', #18811, 5.700000000000001954 ) ;
#19446 = ORIENTED_EDGE ( 'NONE', *, *, #12930, .F. ) ;
#19447 = CARTESIAN_POINT ( 'NONE',  ( -9.000000000000001776, 0.000000000000000000, -35.00000000000000000 ) ) ;
#19448 = CARTESIAN_POINT ( 'NONE',  ( 12.00000000000000355, 0.000000000000000000, 0.000000000000000000 ) ) ;
#19449 = CARTESIAN_POINT ( 'NONE',  ( 5.510910596163084625E-16, 18.00000000000000355, 32.00000000000000000 ) ) ;
#19450 = AXIS2_PLACEMENT_3D ( 'NONE', #7331, #2847, #7539 ) ;
#19451 = CARTESIAN_POINT ( 'NONE',  ( 1.749999999999998002, -12.96210679857804671, 24.89775460606827551 ) ) ;
#19452 = ORIENTED_EDGE ( 'NONE', *, *, #12322, .F. ) ;
#19453 = CARTESIAN_POINT ( 'NONE',  ( 10.96874999795161720, -3.114526743279228072, -3.846120219227966430 ) ) ;
#19454 = CARTESIAN_POINT ( 'NONE',  ( 3.255998204157476206, -17.85806462366060288, 32.00000000000000000 ) ) ;
#19455 = CARTESIAN_POINT ( 'NONE',  ( 2.789999999999999147, -12.59161484032896361, -21.30679549418645280 ) ) ;
#19456 = ADVANCED_FACE ( 'NONE', ( #3764 ), #6943, .F. ) ;
#19457 = VERTEX_POINT ( 'NONE', #17571 ) ;
#19458 = ORIENTED_EDGE ( 'NONE', *, *, #13187, .T. ) ;
#19459 = EDGE_CURVE ( 'NONE', #9124, #19695, #19078, .T. ) ;
#19460 = DIRECTION ( 'NONE',  ( -1.000000000000000000, 1.224646799147353207E-16, 0.000000000000000000 ) ) ;
#19461 = CARTESIAN_POINT ( 'NONE',  ( 10.00000000000000533, -1.185096637661254171, 5.575441324182689229 ) ) ;
#19462 = EDGE_LOOP ( 'NONE', ( #15055, #1356 ) ) ;
#19463 = VECTOR ( 'NONE', #3352, 1000.000000000000000 ) ;
#19464 = DIRECTION ( 'NONE',  ( -0.4067366430758074247, -0.9135454576425977580, 0.000000000000000000 ) ) ;
#19465 = FACE_OUTER_BOUND ( 'NONE', #10860, .T. ) ;
#19466 = ORIENTED_EDGE ( 'NONE', *, *, #7560, .F. ) ;
#19467 = CARTESIAN_POINT ( 'NONE',  ( 1.394999999999998685, -27.76164181293049182, -4.147968289691579713 ) ) ;
#19468 = EDGE_CURVE ( 'NONE', #3180, #8767, #10949, .T. ) ;
#19469 = CYLINDRICAL_SURFACE ( 'NONE', #1960, 2.524999999999995914 ) ;
#19470 = ORIENTED_EDGE ( 'NONE', *, *, #7884, .F. ) ;
#19471 = FACE_OUTER_BOUND ( 'NONE', #5733, .T. ) ;
#19473 = EDGE_CURVE ( 'NONE', #5140, #6183, #16267, .T. ) ;
#19472 = EDGE_CURVE ( 'NONE', #12338, #10379, #12864, .T. ) ;
#19474 = FACE_OUTER_BOUND ( 'NONE', #528, .T. ) ;
#19475 = CARTESIAN_POINT ( 'NONE',  ( 7.812499995903224637, 0.9027913098498568933, -5.699999999999999289 ) ) ;
#19476 = CARTESIAN_POINT ( 'NONE',  ( 9.000000000000000000, 1.102182119232617714E-15, -35.00000000000000000 ) ) ;
#19477 = CIRCLE ( 'NONE', #6061, 1.000000000000002665 ) ;
#19478 = FACE_OUTER_BOUND ( 'NONE', #18797, .T. ) ;
#19479 = VECTOR ( 'NONE', #6307, 1000.000000000000000 ) ;
#19480 = DIRECTION ( 'NONE',  ( 0.000000000000000000, 0.000000000000000000, 1.000000000000000000 ) ) ;
#19481 = VERTEX_POINT ( 'NONE', #15971 ) ;
#19482 = DIRECTION ( 'NONE',  ( -1.000000000000000000, 0.000000000000000000, -0.000000000000000000 ) ) ;
#19483 = DIRECTION ( 'NONE',  ( 0.000000000000000000, 0.000000000000000000, -1.000000000000000000 ) ) ;
#19484 = LINE ( 'NONE', #9092, #11828 ) ;
#19485 = CYLINDRICAL_SURFACE ( 'NONE', #2940, 13.20000000000000284 ) ;
#19486 = CARTESIAN_POINT ( 'NONE',  ( -2.993098736590125853E-16, 4.888101187500000222, -11.84374999795161365 ) ) ;
#19487 = VERTEX_POINT ( 'NONE', #14670 ) ;
#19488 = FACE_OUTER_BOUND ( 'NONE', #13509, .T. ) ;
#19489 = CARTESIAN_POINT ( 'NONE',  ( -41.99999999999999289, 1.999999999999998224, -2.000000000000000000 ) ) ;
#19490 = CIRCLE ( 'NONE', #12474, 24.12539914357697413 ) ;
#19491 = ORIENTED_EDGE ( 'NONE', *, *, #9391, .F. ) ;
#19492 = CARTESIAN_POINT ( 'NONE',  ( 17.96448111170888851, 1.130229351527639148, 32.00000000000000000 ) ) ;
#19493 = AXIS2_PLACEMENT_3D ( 'NONE', #10513, #13506, #8909 ) ;
#19494 = CARTESIAN_POINT ( 'NONE',  ( 12.31249999590322552, -2.849999999999954792, -4.936344801571327601 ) ) ;
#19495 = CARTESIAN_POINT ( 'NONE',  ( 8.968749997951613651, -1.280903732194386579, -4.780397808154273953 ) ) ;
#19496 = LINE ( 'NONE', #7277, #18326 ) ;
#19497 = VERTEX_POINT ( 'NONE', #12972 ) ;
#19498 = CARTESIAN_POINT ( 'NONE',  ( 2.789999999999999147, 24.04302995059966364, -1.991882183130384121 ) ) ;
#19499 = SURFACE_STYLE_FILL_AREA ( #13401 ) ;
#19500 = DIRECTION ( 'NONE',  ( 0.000000000000000000, 0.000000000000000000, -1.000000000000000000 ) ) ;
#19501 = SURFACE_STYLE_FILL_AREA ( #10415 ) ;
#19502 = ORIENTED_EDGE ( 'NONE', *, *, #14486, .T. ) ;
#19503 = CARTESIAN_POINT ( 'NONE',  ( -10.00000000000000000, 0.000000000000000000, 0.000000000000000000 ) ) ;
#19504 = ORIENTED_EDGE ( 'NONE', *, *, #2648, .F. ) ;
#19505 = AXIS2_PLACEMENT_3D ( 'NONE', #9155, #14956, #8856 ) ;
#19506 = AXIS2_PLACEMENT_3D ( 'NONE', #19337, #8641, #14748 ) ;
#19507 = DIRECTION ( 'NONE',  ( 0.000000000000000000, 0.000000000000000000, -1.000000000000000000 ) ) ;
#19508 = CARTESIAN_POINT ( 'NONE',  ( 0.000000000000000000, -1.991882183130148087, -24.04302995059968140 ) ) ;
#19509 = CARTESIAN_POINT ( 'NONE',  ( 13.00000000000000533, -4.611396867937178179, -3.350375938067128967 ) ) ;
#19510 = B_SPLINE_CURVE_WITH_KNOTS ( 'NONE', 3,
 ( #8189, #6282, #18500, #10901, #14197, #18795 ),
 .UNSPECIFIED., .F., .F.,
 ( 4, 2, 4 ),
 ( 4.462636793131339774E-07, 0.001879885123570645012, 0.003759323983461976965 ),
 .UNSPECIFIED. ) ;
#19511 = CARTESIAN_POINT ( 'NONE',  ( -19.00000000000000355, 3.434748899119117294, -2.750000000000002220 ) ) ;
#19512 = ORIENTED_EDGE ( 'NONE', *, *, #10725, .T. ) ;
#19513 = FACE_OUTER_BOUND ( 'NONE', #17266, .T. ) ;
#19514 = CARTESIAN_POINT ( 'NONE',  ( 12.65441706489329299, -3.384649025117529408, 4.627665042997723965 ) ) ;
#19515 = ORIENTED_EDGE ( 'NONE', *, *, #13204, .T. ) ;
#19516 = EDGE_CURVE ( 'NONE', #18746, #1278, #16388, .T. ) ;
#19517 = AXIS2_PLACEMENT_3D ( 'NONE', #757, #17846, #13337 ) ;
#19518 = CARTESIAN_POINT ( 'NONE',  ( -0.7741991708318890497, 4.888101187500000222, -10.96874999795161720 ) ) ;
#19519 = DIRECTION ( 'NONE',  ( 0.000000000000000000, 0.000000000000000000, -1.000000000000000000 ) ) ;
#19520 = EDGE_LOOP ( 'NONE', ( #9867, #6056, #5072, #17173, #5746, #9385 ) ) ;
#19521 = CARTESIAN_POINT ( 'NONE',  ( 5.574407415329170057, 1.493657965219485018, -8.500000000000005329 ) ) ;
#19522 = CARTESIAN_POINT ( 'NONE',  ( -0.000000000000000000, 0.000000000000000000, 0.000000000000000000 ) ) ;
#19523 = FACE_BOUND ( 'NONE', #13702, .T. ) ;
#19524 = ORIENTED_EDGE ( 'NONE', *, *, #7337, .F. ) ;
#19525 = CYLINDRICAL_SURFACE ( 'NONE', #11192, 13.19999999999999929 ) ;
#19526 = VERTEX_POINT ( 'NONE', #19160 ) ;
#19527 = CARTESIAN_POINT ( 'NONE',  ( 2.257825477245772650, 19.66801664102704095, 18.57583492944426951 ) ) ;
#19528 = ORIENTED_EDGE ( 'NONE', *, *, #7757, .F. ) ;
#19529 = CARTESIAN_POINT ( 'NONE',  ( 0.000000000000000000, 0.000000000000000000, -6.527800000000000047 ) ) ;
#19530 = CARTESIAN_POINT ( 'NONE',  ( 1.545624935189822177E-15, 9.165435523385314198, -6.527800000000000047 ) ) ;
#19531 = CARTESIAN_POINT ( 'NONE',  ( -2.246813503491864150, -4.409619785863891472, -13.34374999795161365 ) ) ;
#19532 = CIRCLE ( 'NONE', #372, 1.000000000000004441 ) ;
#19533 = AXIS2_PLACEMENT_3D ( 'NONE', #1781, #9197, #15197 ) ;
#19534 = CARTESIAN_POINT ( 'NONE',  ( 0.7589665283901001480, -3.797536611356509439, 27.31260702007174146 ) ) ;
#19535 = ORIENTED_EDGE ( 'NONE', *, *, #16689, .T. ) ;
#19536 = AXIS2_PLACEMENT_3D ( 'NONE', #2026, #19030, #5322 ) ;
#19537 = DIRECTION ( 'NONE',  ( 1.000000000000000000, 0.000000000000000000, 0.000000000000000000 ) ) ;
#19538 = EDGE_CURVE ( 'NONE', #3728, #5485, #10076, .T. ) ;
#19539 = DIRECTION ( 'NONE',  ( -1.000000000000000000, 0.000000000000000000, -0.000000000000000000 ) ) ;
#19540 =( BOUNDED_CURVE ( )  B_SPLINE_CURVE ( 2, ( #4916, #11120, #8111, #17126, #5102, #6302, #8211, #11216, #5209 ),
 .UNSPECIFIED., .F., .F. ) 
 B_SPLINE_CURVE_WITH_KNOTS ( ( 3, 2, 2, 2, 3 ),
 ( 0.1666819079834116757, 0.2000000000000000111, 0.2500000000000000000, 0.2999999999999999889, 0.3499999999999999778 ),
 .UNSPECIFIED. ) 
 CURVE ( )  GEOMETRIC_REPRESENTATION_ITEM ( )  RATIONAL_B_SPLINE_CURVE ( ( 0.9945256517182512468, 0.9917959799814380917, 1.000000000000000000, 0.9876883405951377704, 1.000000000000000000, 0.9876883405951377704, 1.000000000000000000, 0.9876883405951377704, 1.000000000000000000 ) ) 
 REPRESENTATION_ITEM ( '' )  );
#19541 = ORIENTED_EDGE ( 'NONE', *, *, #7251, .T. ) ;
#19542 = EDGE_CURVE ( 'NONE', #16727, #12097, #15873, .T. ) ;
#19543 = LINE ( 'NONE', #6132, #12821 ) ;
#19544 = AXIS2_PLACEMENT_3D ( 'NONE', #909, #6988, #13110 ) ;
#19545 = CARTESIAN_POINT ( 'NONE',  ( 6.468749997951615427, -3.413342815706642518E-14, 4.888101187500000222 ) ) ;
#19546 = AXIS2_PLACEMENT_3D ( 'NONE', #587, #6959, #9697 ) ;
#19547 = CARTESIAN_POINT ( 'NONE',  ( 5.574407415329170057, 1.493657965219485018, -8.500000000000007105 ) ) ;
#19548 = CIRCLE ( 'NONE', #15741, 1.000000000000004441 ) ;
#19549 = CARTESIAN_POINT ( 'NONE',  ( 0.000000000000000000, 0.000000000000000000, -3.323500000000020993 ) ) ;
#19550 = ORIENTED_EDGE ( 'NONE', *, *, #15946, .T. ) ;
#19551 = CARTESIAN_POINT ( 'NONE',  ( 4.780397808154257078, -1.280903732194453859, -13.96874999795161365 ) ) ;
#19552 = CARTESIAN_POINT ( 'NONE',  ( 0.000000000000000000, 0.000000000000000000, 32.50000000000000000 ) ) ;
#19553 = CARTESIAN_POINT ( 'NONE',  ( -4.781284448697201483, -1.016293382781378485, -12.46874999795161543 ) ) ;
#19554 = DIRECTION ( 'NONE',  ( -1.000000000000000000, 0.000000000000000000, 0.000000000000000000 ) ) ;
#19555 = CIRCLE ( 'NONE', #6767, 4.200000000000000178 ) ;
#19556 = VERTEX_POINT ( 'NONE', #17763 ) ;
#19557 = ORIENTED_EDGE ( 'NONE', *, *, #18158, .T. ) ;
#19558 = DIRECTION ( 'NONE',  ( -0.000000000000000000, -0.000000000000000000, -1.000000000000000000 ) ) ;
#19559 = CARTESIAN_POINT ( 'NONE',  ( 11.96874999795161365, -3.114526743279282250, 3.846120219227923798 ) ) ;
#19560 = VERTEX_POINT ( 'NONE', #4057 ) ;
#19561 = EDGE_CURVE ( 'NONE', #530, #3222, #410, .T. ) ;
#19562 = AXIS2_PLACEMENT_3D ( 'NONE', #17471, #8470, #16077 ) ;
#19563 = DIRECTION ( 'NONE',  ( 0.000000000000000000, -1.000000000000000000, 0.000000000000000000 ) ) ;
#19564 = AXIS2_PLACEMENT_3D ( 'NONE', #15174, #15570, #12468 ) ;
#19565 = ORIENTED_EDGE ( 'NONE', *, *, #840, .T. ) ;
#19566 = DIRECTION ( 'NONE',  ( 1.000000000000000000, 0.000000000000000000, 0.000000000000000000 ) ) ;
#19567 = VECTOR ( 'NONE', #14037, 1000.000000000000114 ) ;
#19568 = DIRECTION ( 'NONE',  ( 0.000000000000000000, 0.000000000000000000, 1.000000000000000000 ) ) ;
#19569 = ADVANCED_FACE ( 'NONE', ( #12773 ), #5525, .T. ) ;
#19570 = ORIENTED_EDGE ( 'NONE', *, *, #2107, .T. ) ;
#19571 = CLOSED_SHELL ( 'NONE', ( #13345, #368, #2448, #16294, #2966, #16309, #10185, #15068, #12467, #9714, #3597, #15028, #8712, #15856, #1490, #16087, #19569, #14041, #17344, #14573, #679, #7143 ) ) ;
#19572 = AXIS2_PLACEMENT_3D ( 'NONE', #8038, #4656, #14154 ) ;
#19573 = ADVANCED_FACE ( 'NONE', ( #17374 ), #3659, .F. ) ;
#19574 = DIRECTION ( 'NONE',  ( 0.000000000000000000, 0.000000000000000000, -1.000000000000000000 ) ) ;
#19575 = CARTESIAN_POINT ( 'NONE',  ( 10.81249999590322375, 5.142044285764749922, -2.620002426024544473 ) ) ;
#19576 = DIRECTION ( 'NONE',  ( -1.000000000000000000, -0.000000000000000000, -0.000000000000000000 ) ) ;
#19577 = VECTOR ( 'NONE', #2208, 1000.000000000000000 ) ;
#19578 = ORIENTED_EDGE ( 'NONE', *, *, #7683, .T. ) ;
#19579 = DIRECTION ( 'NONE',  ( -0.4999999999999979461, -6.047423072554923456E-15, 0.8660254037844398178 ) ) ;
#19580 = SURFACE_STYLE_FILL_AREA ( #7255 ) ;
#19581 = CARTESIAN_POINT ( 'NONE',  ( 0.000000000000000000, -15.74360496233370021, -18.28042085475294698 ) ) ;
#19582 = VERTEX_POINT ( 'NONE', #9058 ) ;
#19583 = EDGE_CURVE ( 'NONE', #9230, #2041, #14162, .T. ) ;
#19584 = DIRECTION ( 'NONE',  ( -0.4999999999999979461, 6.047423072554923456E-15, -0.8660254037844398178 ) ) ;
#19585 = DIRECTION ( 'NONE',  ( 0.000000000000000000, 0.000000000000000000, 1.000000000000000000 ) ) ;
#19586 = AXIS2_PLACEMENT_3D ( 'NONE', #3441, #8726, #13325 ) ;
#19587 = UNCERTAINTY_MEASURE_WITH_UNIT (LENGTH_MEASURE( 1.000000000000000082E-05 ), #4281, 'distance_accuracy_value', 'NONE');
#19588 = CARTESIAN_POINT ( 'NONE',  ( 13.00000000000000533, 5.207209108562852684, -2.318398865532001363 ) ) ;
#19589 = CIRCLE ( 'NONE', #16731, 1.000000000000002665 ) ;
#19590 = CARTESIAN_POINT ( 'NONE',  ( 3.968750000000004441, -6.874076642538978987, 0.000000000000000000 ) ) ;
#19591 = CARTESIAN_POINT ( 'NONE',  ( 0.000000000000000000, 0.000000000000000000, 35.00000000000000000 ) ) ;
#19592 = EDGE_CURVE ( 'NONE', #13120, #13819, #10366, .T. ) ;
#19593 = ORIENTED_EDGE ( 'NONE', *, *, #5470, .F. ) ;
#19594 = EDGE_CURVE ( 'NONE', #16863, #10962, #15769, .T. ) ;
#19595 = CARTESIAN_POINT ( 'NONE',  ( 6.626241948324199882, -16.73597674598852691, -32.00000000000000000 ) ) ;
#19596 = CARTESIAN_POINT ( 'NONE',  ( 12.83455515208547482, -0.2987243419133426281, 5.700000000000001066 ) ) ;
#19597 = COLOUR_RGB ( '', 0.66274510, 0.83137255, 0.94901961) ;
#19598 = EDGE_LOOP ( 'NONE', ( #18167, #7780 ) ) ;
#19599 = CARTESIAN_POINT ( 'NONE',  ( 2.789999999999999147, 2.680914349914567470E-13, -23.06981291497571362 ) ) ;
#19600 = FACE_OUTER_BOUND ( 'NONE', #2955, .T. ) ;
#19601 = CIRCLE ( 'NONE', #7120, 7.937500000000000000 ) ;
#19602 = CARTESIAN_POINT ( 'NONE',  ( -7.937500000000000000, 0.000000000000000000, 0.000000000000000000 ) ) ;
#19603 = DIRECTION ( 'NONE',  ( 0.000000000000000000, 0.000000000000000000, 1.000000000000000000 ) ) ;
#19604 = SHAPE_REPRESENTATION ( 'radial cylindrical roller bearing_iso_ISO 15 RCR - 3712 - 24,SI,NC,24', ( #16724 ), #8276 ) ;
#19605 = ORIENTED_EDGE ( 'NONE', *, *, #2228, .F. ) ;
#19606 = DIRECTION ( 'NONE',  ( 1.000000000000000000, 6.419766481290786633E-33, -0.000000000000000000 ) ) ;
#19607 = CARTESIAN_POINT ( 'NONE',  ( 12.00000000000000355, 0.000000000000000000, -4.000000000000000000 ) ) ;
#19608 = EDGE_CURVE ( 'NONE', #17337, #3073, #17991, .T. ) ;
#19609 = CARTESIAN_POINT ( 'NONE',  ( 0.02436607992776325046, -18.55949924794904504, 16.37294372382852004 ) ) ;
#19610 = ORIENTED_EDGE ( 'NONE', *, *, #9296, .F. ) ;
#19611 = CARTESIAN_POINT ( 'NONE',  ( 0.5958122406255995651, -5.668774803599162304, -15.31249999590322552 ) ) ;
#19612 = EDGE_LOOP ( 'NONE', ( #939, #14852, #5250, #18249 ) ) ;
#19613 = CIRCLE ( 'NONE', #9735, 28.06981291497571362 ) ;
#19614 = CARTESIAN_POINT ( 'NONE',  ( 6.968749997951614539, -0.7741991708319229115, 4.888101187499994893 ) ) ;
#19615 = CARTESIAN_POINT ( 'NONE',  ( -7.646929282184496191E-14, 5.456611084822186264, -23.69897269326672884 ) ) ;
#19616 = CARTESIAN_POINT ( 'NONE',  ( 1.749999999999998002, 27.68468304288259318, 4.633866840649019103 ) ) ;
#19617 = ADVANCED_FACE ( 'NONE', ( #10559 ), #4547, .F. ) ;
#19618 = CARTESIAN_POINT ( 'NONE',  ( -1.016293382781411569, 4.781284448697194378, -7.843749997951614539 ) ) ;
#19619 = ADVANCED_FACE ( 'NONE', ( #13353 ), #10021, .T. ) ;
#19620 = ORIENTED_EDGE ( 'NONE', *, *, #237, .F. ) ;
#19621 = AXIS2_PLACEMENT_3D ( 'NONE', #11355, #3741, #8142 ) ;
#19622 = DIRECTION ( 'NONE',  ( -1.000000000000000000, 0.000000000000000000, 0.000000000000000000 ) ) ;
#19623 = CARTESIAN_POINT ( 'NONE',  ( 0.7589665283900991488, 27.31260702007175567, 3.797536611356412628 ) ) ;
#19624 = ORIENTED_EDGE ( 'NONE', *, *, #17074, .T. ) ;
#19625 = VECTOR ( 'NONE', #7230, 1000.000000000000000 ) ;
#19626 = CARTESIAN_POINT ( 'NONE',  ( -3.499494075959816541, 3.499494075959816541, -9.343749997951615427 ) ) ;
#19627 = CARTESIAN_POINT ( 'NONE',  ( 2.718131864678290821, 25.22589920183360945, -2.577209017047097372 ) ) ;
#19628 = EDGE_LOOP ( 'NONE', ( #13244, #3553, #8169, #4099, #16890, #13112, #552, #14938 ) ) ;
#19629 = CARTESIAN_POINT ( 'NONE',  ( -5.000000000000000000, -2.000000000000001332, 41.99999999999999289 ) ) ;
#19630 = CARTESIAN_POINT ( 'NONE',  ( 14.34374999795161365, -1.280903732194453637, 4.780397808154257078 ) ) ;
#19631 = FACE_OUTER_BOUND ( 'NONE', #7673, .T. ) ;
#19632 = CIRCLE ( 'NONE', #18674, 1.000000000000000888 ) ;
#19633 = ADVANCED_FACE ( 'NONE', ( #2741 ), #15438, .T. ) ;
#19634 = ORIENTED_EDGE ( 'NONE', *, *, #5280, .F. ) ;
#19635 = DIRECTION ( 'NONE',  ( 0.000000000000000000, 0.000000000000000000, 1.000000000000000000 ) ) ;
#19636 = VERTEX_POINT ( 'NONE', #19451 ) ;
#19637 = DIRECTION ( 'NONE',  ( 1.000000000000000000, 6.419766481290786633E-33, -0.000000000000000000 ) ) ;
#19638 = ORIENTED_EDGE ( 'NONE', *, *, #1813, .F. ) ;
#19639 = CARTESIAN_POINT ( 'NONE',  ( 0.5321745087963410947, 24.44564404695860205, -11.58891744060082019 ) ) ;
#19640 = CARTESIAN_POINT ( 'NONE',  ( 0.000000000000000000, 7.909232158575156824, -21.81711360614291806 ) ) ;
#19641 = CARTESIAN_POINT ( 'NONE',  ( -3.499494075959840078, -3.499494075959791672, -13.96874999795161365 ) ) ;
#19642 = FACE_OUTER_BOUND ( 'NONE', #4132, .T. ) ;
#19643 = CIRCLE ( 'NONE', #13890, 3.968750000000000000 ) ;
#19644 = CARTESIAN_POINT ( 'NONE',  ( 13.00000000000000178, 0.7793280607715257213, 4.825575716215943167 ) ) ;
#19645 = EDGE_CURVE ( 'NONE', #15548, #18748, #19264, .T. ) ;
#19646 = VERTEX_POINT ( 'NONE', #19549 ) ;
#19647 = CARTESIAN_POINT ( 'NONE',  ( 2.765633920072238183, -5.391175441198789109, 24.15498966839961170 ) ) ;
#19648 = FACE_OUTER_BOUND ( 'NONE', #12632, .T. ) ;
#19649 = ORIENTED_EDGE ( 'NONE', *, *, #18394, .F. ) ;
#19650 = ADVANCED_FACE ( 'NONE', ( #5843, #4354 ), #4451, .F. ) ;
#19651 = DIRECTION ( 'NONE',  ( 1.000000000000000000, 0.000000000000000000, 0.000000000000000000 ) ) ;
#19652 = ORIENTED_EDGE ( 'NONE', *, *, #6979, .F. ) ;
#19653 = AXIS2_PLACEMENT_3D ( 'NONE', #17289, #14392, #8079 ) ;
#19654 = FACE_OUTER_BOUND ( 'NONE', #7062, .T. ) ;
#19656 = CARTESIAN_POINT ( 'NONE',  ( 3.814044456245474279, -4.235925505221167064, -12.00000000000000533 ) ) ;
#19655 = VECTOR ( 'NONE', #11447, 1000.000000000000000 ) ;
#19657 = CARTESIAN_POINT ( 'NONE',  ( -34.92499999999994742, 4.898587196589412829E-16, -4.000000000000000000 ) ) ;
#19658 = EDGE_LOOP ( 'NONE', ( #9931, #8050, #7809 ) ) ;
#19659 = CARTESIAN_POINT ( 'NONE',  ( -2.300000000000000711, 7.592810154713614487E-16, 6.200000000000020606 ) ) ;
#19660 = DIRECTION ( 'NONE',  ( 0.000000000000000000, 0.000000000000000000, -0.9999999999999998890 ) ) ;
#19661 = CARTESIAN_POINT ( 'NONE',  ( 1.016293382781377819, -4.781284448697200595, -7.468749997951615427 ) ) ;
#19662 = ORIENTED_EDGE ( 'NONE', *, *, #6844, .T. ) ;
#19663 = ORIENTED_EDGE ( 'NONE', *, *, #2231, .F. ) ;
#19664 = CARTESIAN_POINT ( 'NONE',  ( 2.789999999999999147, 0.000000000000000000, 0.000000000000000000 ) ) ;
#19665 = CARTESIAN_POINT ( 'NONE',  ( 2.031033471609899888, -3.797536611356125746, -27.31260702007179830 ) ) ;
#19666 = EDGE_CURVE ( 'NONE', #18724, #10514, #1353, .T. ) ;
#19667 = ORIENTED_EDGE ( 'NONE', *, *, #17565, .F. ) ;
#19668 = VECTOR ( 'NONE', #8032, 1000.000000000000000 ) ;
#19669 = DIRECTION ( 'NONE',  ( 0.000000000000000000, 0.000000000000000000, -1.000000000000000000 ) ) ;
#19670 = ORIENTED_EDGE ( 'NONE', *, *, #4418, .T. ) ;
#19671 = VECTOR ( 'NONE', #19036, 1000.000000000000000 ) ;
#19672 = DIRECTION ( 'NONE',  ( 1.000000000000000000, 0.000000000000000000, 0.000000000000000000 ) ) ;
#19673 = ORIENTED_EDGE ( 'NONE', *, *, #16674, .T. ) ;
#19674 = FACE_OUTER_BOUND ( 'NONE', #8904, .T. ) ;
#19675 = CARTESIAN_POINT ( 'NONE',  ( 9.312499995903225525, 3.350375938067097437, -4.611396867937201272 ) ) ;
#19676 = EDGE_CURVE ( 'NONE', #19176, #676, #14491, .T. ) ;
#19677 = EDGE_CURVE ( 'NONE', #15929, #1471, #17592, .T. ) ;
#19678 = DIRECTION ( 'NONE',  ( 1.000000000000000000, 0.000000000000000000, 0.000000000000000000 ) ) ;
#19679 = CIRCLE ( 'NONE', #11063, 2.524999999999995470 ) ;
#19680 = EDGE_LOOP ( 'NONE', ( #5918, #16670, #19541, #6046 ) ) ;
#19681 = LINE ( 'NONE', #4473, #545 ) ;
#19682 = DIRECTION ( 'NONE',  ( -0.000000000000000000, -0.000000000000000000, 1.000000000000000000 ) ) ;
#19683 = TOROIDAL_SURFACE ( 'NONE', #2427, 8.800000000000023803, 0.1999999999999994282 ) ;
#19684 = ORIENTED_EDGE ( 'NONE', *, *, #19103, .T. ) ;
#19685 = CARTESIAN_POINT ( 'NONE',  ( 2.789999999999999147, 16.37294372382858398, 18.55949924794898465 ) ) ;
#19686 = FACE_BOUND ( 'NONE', #5517, .T. ) ;
#19687 = CARTESIAN_POINT ( 'NONE',  ( 2.000000000000001776, 8.327598234202001119E-16, 6.799999999999999822 ) ) ;
#19688 = EDGE_CURVE ( 'NONE', #18545, #16477, #1251, .T. ) ;
#19689 = DIRECTION ( 'NONE',  ( 0.000000000000000000, 0.000000000000000000, 1.000000000000000000 ) ) ;
#19690 = CARTESIAN_POINT ( 'NONE',  ( 13.00000000000000000, 4.333424887443004359, 2.261628166637590365 ) ) ;
#19691 = ORIENTED_EDGE ( 'NONE', *, *, #2051, .T. ) ;
#19692 = DIRECTION ( 'NONE',  ( -1.000000000000000000, -0.000000000000000000, -0.000000000000000000 ) ) ;
#19693 = CARTESIAN_POINT ( 'NONE',  ( -2.695436003842674122, 4.150607464521828938, -12.96874999795161543 ) ) ;
#19694 = AXIS2_PLACEMENT_3D ( 'NONE', #14694, #7254, #7460 ) ;
#19695 = VERTEX_POINT ( 'NONE', #7328 ) ;
#19696 = CARTESIAN_POINT ( 'NONE',  ( 6.468749997951615427, -4.233219804643852946, -2.444050593750049849 ) ) ;
#19697 = AXIS2_PLACEMENT_3D ( 'NONE', #11086, #5171, #6459 ) ;
#19698 = CARTESIAN_POINT ( 'NONE',  ( -2.000000000000000000, -2.000000000000001776, 37.99999999999999289 ) ) ;
#19699 = CARTESIAN_POINT ( 'NONE',  ( -7.937500000000000000, 3.841717848563040771, -0.4950406553165774826 ) ) ;
#19700 = CARTESIAN_POINT ( 'NONE',  ( 12.66727757604273386, -4.360680574150373717E-16, 5.700000000000001066 ) ) ;
#19701 = PRODUCT_DEFINITION ( 'UNKNOWN', '', #8291, #17407 ) ;
#19702 = ORIENTED_EDGE ( 'NONE', *, *, #19004, .T. ) ;
#19703 = FACE_OUTER_BOUND ( 'NONE', #17416, .T. ) ;
#19704 = DIRECTION ( 'NONE',  ( 0.000000000000000000, 0.000000000000000000, -1.000000000000000000 ) ) ;
#19705 = VERTEX_POINT ( 'NONE', #1453 ) ;
#19706 = CARTESIAN_POINT ( 'NONE',  ( 0.5958122406255970116, -5.668774803599162304, 0.000000000000000000 ) ) ;
#19707 = CIRCLE ( 'NONE', #2776, 1.000000000000003553 ) ;
#19708 = CARTESIAN_POINT ( 'NONE',  ( 10.96874999795161720, -1.773574444220757274, 4.620319390059819398 ) ) ;
#19709 = CARTESIAN_POINT ( 'NONE',  ( -0.5109457054261112852, 4.861323657744413218, -14.46874999795161720 ) ) ;
#19710 = VECTOR ( 'NONE', #17015, 1000.000000000000000 ) ;
#19711 = EDGE_CURVE ( 'NONE', #3728, #16926, #6162, .T. ) ;
#19712 = CARTESIAN_POINT ( 'NONE',  ( 11.96874999795161365, 4.888101187500000222, 0.7741991708318884946 ) ) ;
#19713 = EDGE_CURVE ( 'NONE', #10348, #10842, #1713, .T. ) ;
#19714 = DIRECTION ( 'NONE',  ( -1.000000000000000000, -0.000000000000000000, -0.000000000000000000 ) ) ;
#19715 = DIRECTION ( 'NONE',  ( -0.8660254037844419273, 0.4999999999999944489, 0.000000000000000000 ) ) ;
#19716 = ORIENTED_EDGE ( 'NONE', *, *, #9672, .T. ) ;
#19717 = CARTESIAN_POINT ( 'NONE',  ( -4.620319390059841602, -1.773574444220693325, -12.34374999795161543 ) ) ;
#19718 = DIRECTION ( 'NONE',  ( -1.000000000000000000, -0.000000000000000000, -0.000000000000000000 ) ) ;
#19719 = ORIENTED_EDGE ( 'NONE', *, *, #443, .F. ) ;
#19720 = EDGE_CURVE ( 'NONE', #8429, #4625, #2644, .T. ) ;
#19721 = CIRCLE ( 'NONE', #18453, 28.06981291497571007 ) ;
#19722 = AXIS2_PLACEMENT_3D ( 'NONE', #7026, #17753, #13152 ) ;
#19723 = CARTESIAN_POINT ( 'NONE',  ( -4.888101187500000222, 0.000000000000000000, -6.843749997951615427 ) ) ;
#19724 = ORIENTED_EDGE ( 'NONE', *, *, #14674, .T. ) ;
#19725 = CARTESIAN_POINT ( 'NONE',  ( -1.773574444220725077, 4.620319390059829168, -7.343749997951615427 ) ) ;
#19726 = EDGE_CURVE ( 'NONE', #15015, #5395, #3885, .T. ) ;
#19727 = CARTESIAN_POINT ( 'NONE',  ( -4.409619785863906571, 2.246813503491833508, -7.968749997951616315 ) ) ;
#19728 = EDGE_LOOP ( 'NONE', ( #16751, #4556, #610, #708, #19702, #13158 ) ) ;
#19729 = FACE_OUTER_BOUND ( 'NONE', #8133, .T. ) ;
#19730 = ORIENTED_EDGE ( 'NONE', *, *, #12598, .T. ) ;
#19731 = FACE_OUTER_BOUND ( 'NONE', #4773, .T. ) ;
#19732 = ORIENTED_EDGE ( 'NONE', *, *, #17523, .F. ) ;
#19733 = DIRECTION ( 'NONE',  ( -0.000000000000000000, -0.000000000000000000, 1.000000000000000000 ) ) ;
#19734 = DIRECTION ( 'NONE',  ( 0.000000000000000000, -1.000000000000000000, 0.000000000000000000 ) ) ;
#19735 = CARTESIAN_POINT ( 'NONE',  ( 0.006931111373679591826, -22.53293026234497276, -9.685942809247297447 ) ) ;
#19736 = CARTESIAN_POINT ( 'NONE',  ( 9.468749997951615427, -4.465502636338009701, -1.988169868018624609 ) ) ;
#19737 = DIRECTION ( 'NONE',  ( -1.000000000000000000, 0.000000000000000000, -0.000000000000000000 ) ) ;
#19738 = VECTOR ( 'NONE', #4808, 1000.000000000000000 ) ;
#19739 = ORIENTED_EDGE ( 'NONE', *, *, #17881, .F. ) ;
#19740 = DIRECTION ( 'NONE',  ( 0.000000000000000000, 0.000000000000000000, 1.000000000000000000 ) ) ;
#19741 = EDGE_CURVE ( 'NONE', #10790, #7654, #5014, .T. ) ;
#19742 = ORIENTED_EDGE ( 'NONE', *, *, #4613, .T. ) ;
#19743 = CARTESIAN_POINT ( 'NONE',  ( 0.07181523211953064201, -23.19431517146941246, 10.24584646439529756 ) ) ;
#19744 = CARTESIAN_POINT ( 'NONE',  ( 0.000000000000000000, 0.000000000000000000, 0.000000000000000000 ) ) ;
#19745 = ADVANCED_BREP_SHAPE_REPRESENTATION ( '', ( #9397, #16724 ), #5229 ) ;
#19746 = VECTOR ( 'NONE', #16474, 1000.000000000000000 ) ;
#19747 = ORIENTED_EDGE ( 'NONE', *, *, #3788, .T. ) ;
#19748 = LINE ( 'NONE', #8755, #9950 ) ;
#19749 = CARTESIAN_POINT ( 'NONE',  ( 1.493657965219485462, -5.574407415329169169, -13.50000000000000533 ) ) ;
#19750 = CARTESIAN_POINT ( 'NONE',  ( -30.00000000000000000, -1.925929944387235853E-31, 0.000000000000000000 ) ) ;
#19751 = ORIENTED_EDGE ( 'NONE', *, *, #2082, .F. ) ;
#19752 = CARTESIAN_POINT ( 'NONE',  ( 3.270778111535338262, 3.632567103900523620, -10.46874999795161720 ) ) ;
#19753 =( NAMED_UNIT ( * ) PLANE_ANGLE_UNIT ( ) SI_UNIT ( $, .RADIAN. ) );
#19754 = DIRECTION ( 'NONE',  ( -0.4999999999999920619, 0.8660254037844432595, 0.000000000000000000 ) ) ;
#19755 = DIRECTION ( 'NONE',  ( -1.000000000000000000, 0.000000000000000000, 0.000000000000000000 ) ) ;
#19756 = EDGE_LOOP ( 'NONE', ( #8041, #8247 ) ) ;
#19757 = VERTEX_POINT ( 'NONE', #8115 ) ;
#19758 = DIRECTION ( 'NONE',  ( 1.000000000000000000, 0.000000000000000000, 0.000000000000000000 ) ) ;
#19759 = CARTESIAN_POINT ( 'NONE',  ( 9.343749997951615427, 3.499494075959816541, -3.499494075959816541 ) ) ;
#19760 = VERTEX_POINT ( 'NONE', #11330 ) ;
#19761 = CIRCLE ( 'NONE', #14666, 28.06981291497571362 ) ;
#19762 = PLANE ( 'NONE',  #7838 ) ;
#19763 = ORIENTED_EDGE ( 'NONE', *, *, #18623, .T. ) ;
#19764 = DIRECTION ( 'NONE',  ( 1.000000000000000000, 0.000000000000000000, 0.000000000000000000 ) ) ;
#19765 = ORIENTED_EDGE ( 'NONE', *, *, #12844, .T. ) ;
#19766 = PRODUCT_DEFINITION_FORMATION_WITH_SPECIFIED_SOURCE ( 'ANY', '', #3624, .NOT_KNOWN. ) ;
#19767 = EDGE_CURVE ( 'NONE', #17943, #4963, #2015, .T. ) ;
#19768 = DIRECTION ( 'NONE',  ( -1.000000000000000000, -6.419766481290786633E-33, 0.000000000000000000 ) ) ;
#19769 = DIRECTION ( 'NONE',  ( 1.000000000000000000, 0.000000000000000000, 0.000000000000000000 ) ) ;
#19770 = CARTESIAN_POINT ( 'NONE',  ( 2.620002426024508502, -5.142044285764769462, -10.81249999590322375 ) ) ;
#19771 = AXIS2_PLACEMENT_3D ( 'NONE', #3443, #9555, #7934 ) ;
#19772 = EDGE_LOOP ( 'NONE', ( #18716, #8454, #16127, #13347, #8361 ) ) ;
#19773 = CARTESIAN_POINT ( 'NONE',  ( -15.00000000000000355, -3.434748899119117294, -2.750000000000002220 ) ) ;
#19774 = CARTESIAN_POINT ( 'NONE',  ( 0.000000000000000000, 0.000000000000000000, -0.6113687067993561763 ) ) ;
#19775 = EDGE_LOOP ( 'NONE', ( #6175, #14589, #4463, #13419 ) ) ;
#19776 = DIRECTION ( 'NONE',  ( -1.000000000000000000, 0.000000000000000000, 0.000000000000000000 ) ) ;
#19777 = DIRECTION ( 'NONE',  ( 0.000000000000000000, 0.000000000000000000, 1.000000000000000000 ) ) ;
#19778 = CARTESIAN_POINT ( 'NONE',  ( 1.039999999999996483, -27.76164181293054511, 4.147968289691193355 ) ) ;
#19779 = CARTESIAN_POINT ( 'NONE',  ( -18.68117051311639543, -3.372863662543042818, -35.00000000000000000 ) ) ;
#19780 = CARTESIAN_POINT ( 'NONE',  ( 1.999999999999998668, -8.000000000000003553, 41.99999999999999289 ) ) ;
#19781 = ORIENTED_EDGE ( 'NONE', *, *, #14369, .F. ) ;
#19782 = CARTESIAN_POINT ( 'NONE',  ( 13.34374999795161365, 4.409619785863906571, 2.246813503491833508 ) ) ;
#19783 = NEXT_ASSEMBLY_USAGE_OCCURRENCE ( 'NAUO1', ' ', ' ', #19701, #8823, $ ) ;
#19784 = NEXT_ASSEMBLY_USAGE_OCCURRENCE ( 'NAUO2', ' ', ' ', #19701, #11510, $ ) ;
#19785 = NEXT_ASSEMBLY_USAGE_OCCURRENCE ( 'NAUO3', ' ', ' ', #19701, #2339, $ ) ;
#19786 = NEXT_ASSEMBLY_USAGE_OCCURRENCE ( 'NAUO4', ' ', ' ', #19701, #12983, $ ) ;
#19787 = NEXT_ASSEMBLY_USAGE_OCCURRENCE ( 'NAUO5', ' ', ' ', #19701, #16784, $ ) ;
#19788 = NEXT_ASSEMBLY_USAGE_OCCURRENCE ( 'NAUO6', ' ', ' ', #19701, #16784, $ ) ;
#19789 = NEXT_ASSEMBLY_USAGE_OCCURRENCE ( 'NAUO7', ' ', ' ', #19701, #7325, $ ) ;
#19790 = NEXT_ASSEMBLY_USAGE_OCCURRENCE ( 'NAUO8', ' ', ' ', #19701, #10899, $ ) ;
#19791 = NEXT_ASSEMBLY_USAGE_OCCURRENCE ( 'NAUO9', ' ', ' ', #19701, #10899, $ ) ;
#19792 = NEXT_ASSEMBLY_USAGE_OCCURRENCE ( 'NAUO10', ' ', ' ', #19701, #8091, $ ) ;
#19793 = NEXT_ASSEMBLY_USAGE_OCCURRENCE ( 'NAUO11', ' ', ' ', #19701, #396, $ ) ;
#19794 = NEXT_ASSEMBLY_USAGE_OCCURRENCE ( 'NAUO12', ' ', ' ', #19701, #12622, $ ) ;
#19795 = NEXT_ASSEMBLY_USAGE_OCCURRENCE ( 'NAUO13', ' ', ' ', #19701, #9076, $ ) ;
#19796 = NEXT_ASSEMBLY_USAGE_OCCURRENCE ( 'NAUO14', ' ', ' ', #19701, #1614, $ ) ;
#19797 = NEXT_ASSEMBLY_USAGE_OCCURRENCE ( 'NAUO15', ' ', ' ', #19701, #2224, $ ) ;
#19798 = NEXT_ASSEMBLY_USAGE_OCCURRENCE ( 'NAUO16', ' ', ' ', #19701, #2224, $ ) ;
#19799 = NEXT_ASSEMBLY_USAGE_OCCURRENCE ( 'NAUO17', ' ', ' ', #19701, #7470, $ ) ;
#19800 = NEXT_ASSEMBLY_USAGE_OCCURRENCE ( 'NAUO18', ' ', ' ', #19701, #2224, $ ) ;
ENDSEC;
END-ISO-10303-21;
